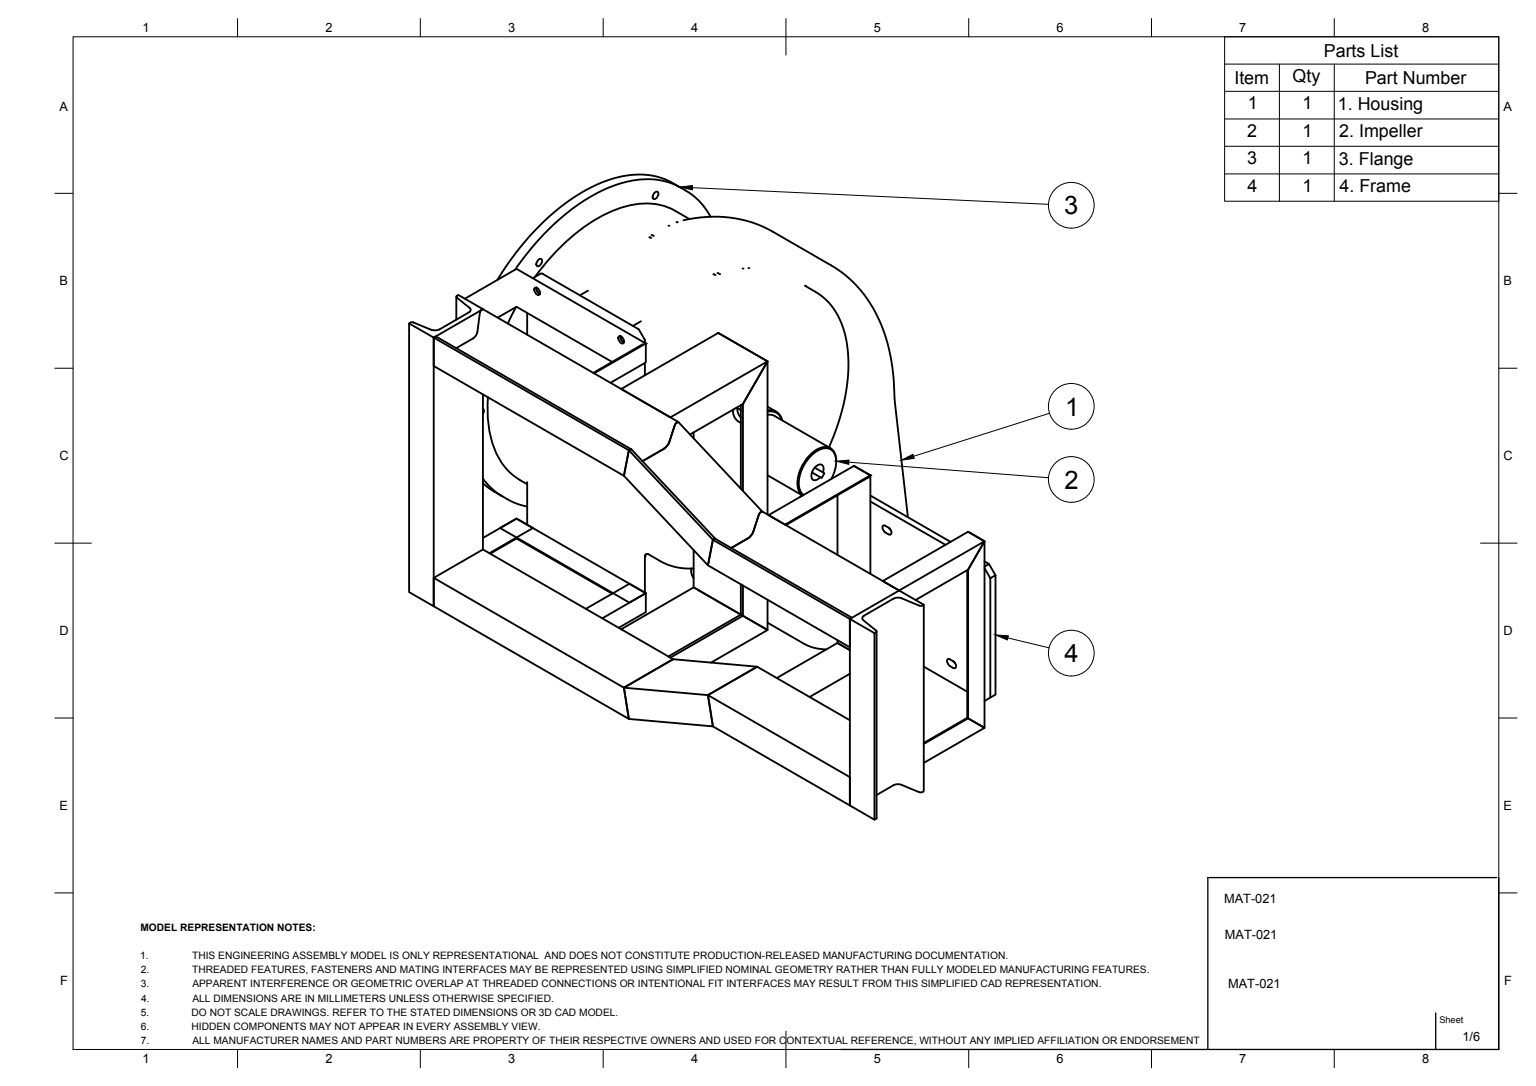
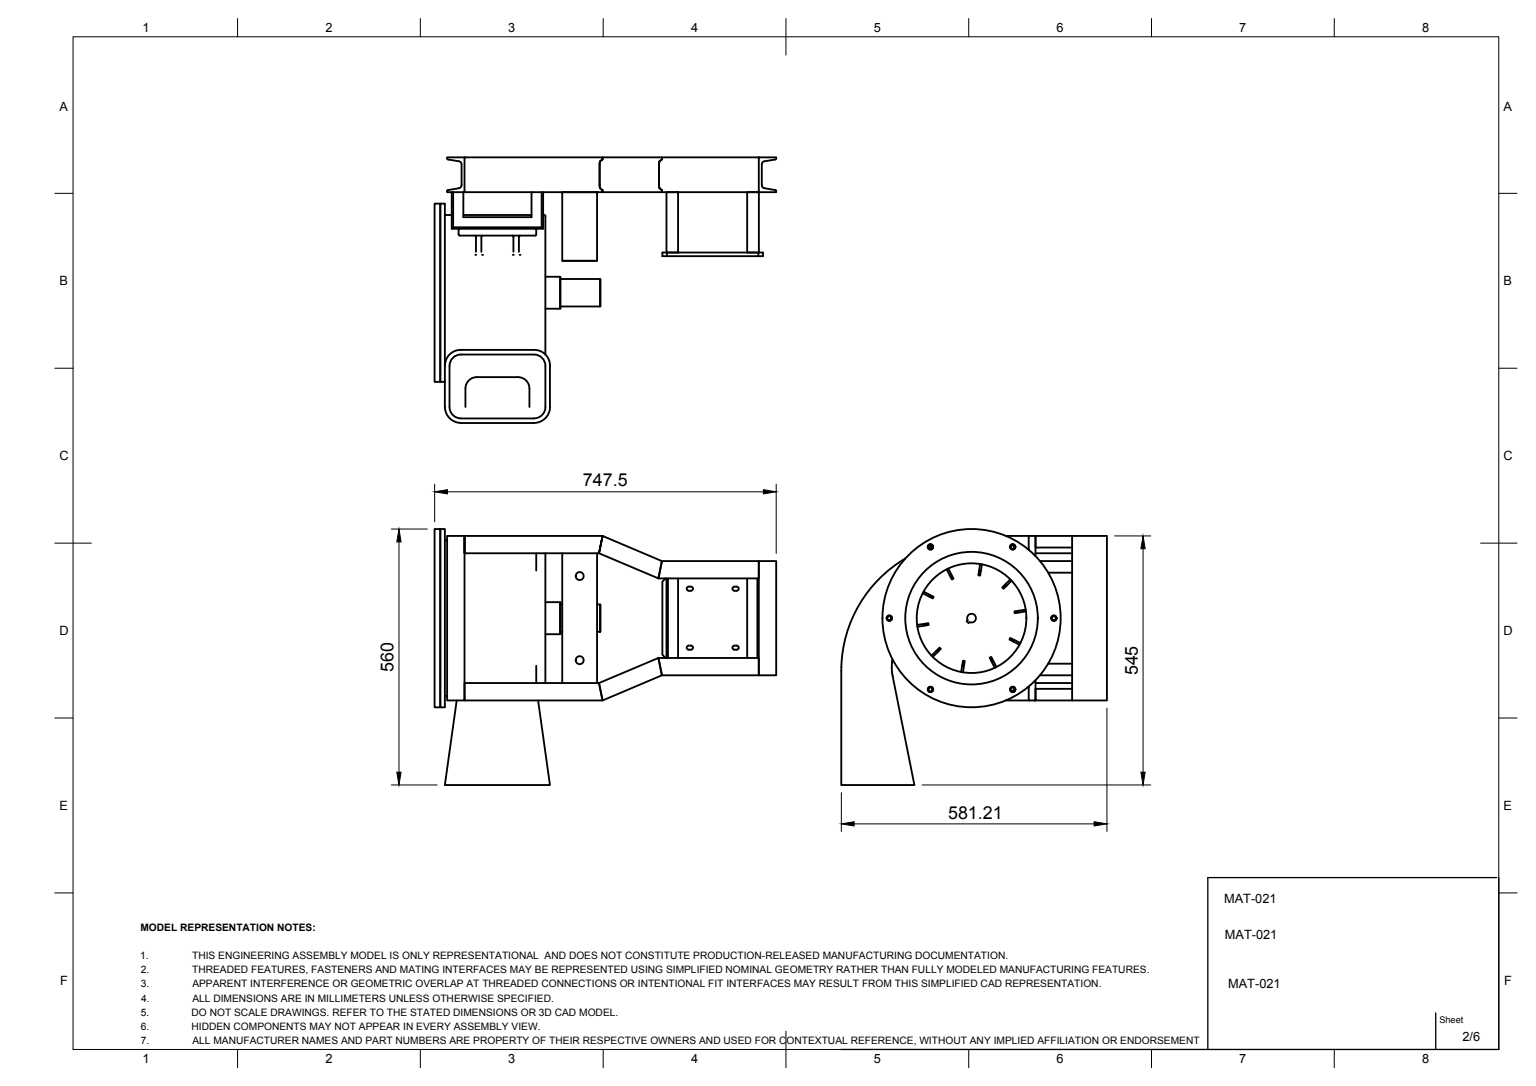
ISO-10303-21;
HEADER;
/* Generated by software containing ST-Developer
 * from STEP Tools, Inc. (www.steptools.com) 
 */

FILE_DESCRIPTION(
/* description */ ('STEP AP214'),
/* implementation_level */ '2;1');

FILE_NAME(
/* name */ 'MAT-021.step',
/* time_stamp */ '2026-11-14T06:27:21-08:00',
/* author */ (''),
/* organization */ (''),
/* preprocessor_version */ 'ST-DEVELOPER v20.2',
/* originating_system */ 'Autodesk Translation Framework v15.17.0.0',
/* authorisation */ '');

FILE_SCHEMA (('AUTOMOTIVE_DESIGN { 1 0 10303 214 3 1 1 }'));
ENDSEC;

DATA;
#10=MECHANICAL_DESIGN_GEOMETRIC_PRESENTATION_REPRESENTATION('',(#35,#36,
#37,#38,#39,#40,#41,#42,#43,#44,#45,#46,#47,#48,#49,#50,#51,#52,#53,#54,
#55,#56,#57,#58,#59,#60,#61),#27541);
#11=ITEM_DEFINED_TRANSFORMATION($,$,#11896,#13173);
#12=ITEM_DEFINED_TRANSFORMATION($,$,#12424,#13174);
#13=ITEM_DEFINED_TRANSFORMATION($,$,#12619,#13175);
#14=ITEM_DEFINED_TRANSFORMATION($,$,#12666,#13176);
#15=(
REPRESENTATION_RELATIONSHIP($,$,#27561,#27560)
REPRESENTATION_RELATIONSHIP_WITH_TRANSFORMATION(#11)
SHAPE_REPRESENTATION_RELATIONSHIP()
);
#16=(
REPRESENTATION_RELATIONSHIP($,$,#27562,#27560)
REPRESENTATION_RELATIONSHIP_WITH_TRANSFORMATION(#12)
SHAPE_REPRESENTATION_RELATIONSHIP()
);
#17=(
REPRESENTATION_RELATIONSHIP($,$,#27563,#27560)
REPRESENTATION_RELATIONSHIP_WITH_TRANSFORMATION(#13)
SHAPE_REPRESENTATION_RELATIONSHIP()
);
#18=(
REPRESENTATION_RELATIONSHIP($,$,#27564,#27560)
REPRESENTATION_RELATIONSHIP_WITH_TRANSFORMATION(#14)
SHAPE_REPRESENTATION_RELATIONSHIP()
);
#19=CONTEXT_DEPENDENT_SHAPE_REPRESENTATION(#15,#27556);
#20=CONTEXT_DEPENDENT_SHAPE_REPRESENTATION(#16,#27557);
#21=CONTEXT_DEPENDENT_SHAPE_REPRESENTATION(#17,#27558);
#22=CONTEXT_DEPENDENT_SHAPE_REPRESENTATION(#18,#27559);
#23=NEXT_ASSEMBLY_USAGE_OCCURRENCE('1. Housing:1','1. Housing:1',
'1. Housing:1',#27566,#27567,'1. Housing:1');
#24=NEXT_ASSEMBLY_USAGE_OCCURRENCE('2. Impeller:1','2. Impeller:1',
'2. Impeller:1',#27566,#27568,'2. Impeller:1');
#25=NEXT_ASSEMBLY_USAGE_OCCURRENCE('3. Flange:1','3. Flange:1',
'3. Flange:1',#27566,#27569,'3. Flange:1');
#26=NEXT_ASSEMBLY_USAGE_OCCURRENCE('4. Frame:1','4. Frame:1',
'4. Frame:1',#27566,#27570,'4. Frame:1');
#27=SHAPE_REPRESENTATION_RELATIONSHIP('SRR','None',#27561,#31);
#28=SHAPE_REPRESENTATION_RELATIONSHIP('SRR','None',#27562,#32);
#29=SHAPE_REPRESENTATION_RELATIONSHIP('SRR','None',#27563,#33);
#30=SHAPE_REPRESENTATION_RELATIONSHIP('SRR','None',#27564,#34);
#31=ADVANCED_BREP_SHAPE_REPRESENTATION('',(#62),#27537);
#32=ADVANCED_BREP_SHAPE_REPRESENTATION('',(#63),#27538);
#33=ADVANCED_BREP_SHAPE_REPRESENTATION('',(#64),#27539);
#34=ADVANCED_BREP_SHAPE_REPRESENTATION('',(#65,#66,#67,#68,#69,#70,#71,
#72,#73,#74,#75,#76,#77,#78,#79,#80,#81,#82,#83,#84,#85,#86,#87,#88),#27540);
#35=STYLED_ITEM('',(#27590),#62);
#36=STYLED_ITEM('',(#27591),#63);
#37=STYLED_ITEM('',(#27592),#64);
#38=STYLED_ITEM('',(#27590),#65);
#39=STYLED_ITEM('',(#27590),#66);
#40=STYLED_ITEM('',(#27590),#67);
#41=STYLED_ITEM('',(#27590),#68);
#42=STYLED_ITEM('',(#27590),#69);
#43=STYLED_ITEM('',(#27590),#70);
#44=STYLED_ITEM('',(#27590),#71);
#45=STYLED_ITEM('',(#27590),#72);
#46=STYLED_ITEM('',(#27590),#73);
#47=STYLED_ITEM('',(#27590),#74);
#48=STYLED_ITEM('',(#27590),#75);
#49=STYLED_ITEM('',(#27590),#76);
#50=STYLED_ITEM('',(#27590),#77);
#51=STYLED_ITEM('',(#27590),#78);
#52=STYLED_ITEM('',(#27590),#79);
#53=STYLED_ITEM('',(#27590),#80);
#54=STYLED_ITEM('',(#27590),#81);
#55=STYLED_ITEM('',(#27590),#82);
#56=STYLED_ITEM('',(#27590),#83);
#57=STYLED_ITEM('',(#27590),#84);
#58=STYLED_ITEM('',(#27590),#85);
#59=STYLED_ITEM('',(#27590),#86);
#60=STYLED_ITEM('',(#27590),#87);
#61=STYLED_ITEM('',(#27590),#88);
#62=MANIFOLD_SOLID_BREP('Body1',#11823);
#63=MANIFOLD_SOLID_BREP('Body1',#11824);
#64=MANIFOLD_SOLID_BREP('Body1',#11825);
#65=MANIFOLD_SOLID_BREP('Body1',#11826);
#66=MANIFOLD_SOLID_BREP('Body2',#11827);
#67=MANIFOLD_SOLID_BREP('Body3',#11828);
#68=MANIFOLD_SOLID_BREP('Body4',#11829);
#69=MANIFOLD_SOLID_BREP('Body5',#11830);
#70=MANIFOLD_SOLID_BREP('Body6',#11831);
#71=MANIFOLD_SOLID_BREP('Body7',#11832);
#72=MANIFOLD_SOLID_BREP('Body8',#11833);
#73=MANIFOLD_SOLID_BREP('Body9',#11834);
#74=MANIFOLD_SOLID_BREP('Body10',#11835);
#75=MANIFOLD_SOLID_BREP('Body11',#11836);
#76=MANIFOLD_SOLID_BREP('Body12',#11837);
#77=MANIFOLD_SOLID_BREP('Body13',#11838);
#78=MANIFOLD_SOLID_BREP('Body14',#11839);
#79=MANIFOLD_SOLID_BREP('Body15',#11840);
#80=MANIFOLD_SOLID_BREP('Body16',#11841);
#81=MANIFOLD_SOLID_BREP('Body17',#11842);
#82=MANIFOLD_SOLID_BREP('Body18',#11843);
#83=MANIFOLD_SOLID_BREP('Body19',#11844);
#84=MANIFOLD_SOLID_BREP('Body20',#11845);
#85=MANIFOLD_SOLID_BREP('Body21',#11846);
#86=MANIFOLD_SOLID_BREP('Body22',#11847);
#87=MANIFOLD_SOLID_BREP('Body23',#11848);
#88=MANIFOLD_SOLID_BREP('Body24',#11849);
#89=(
BOUNDED_SURFACE()
B_SPLINE_SURFACE(3,2,((#19385,#19386,#19387),(#19388,#19389,#19390),(#19391,
#19392,#19393),(#19394,#19395,#19396)),.UNSPECIFIED.,.F.,.F.,.F.)
B_SPLINE_SURFACE_WITH_KNOTS((4,4),(3,3),(4.8580615908835,4.90978454023457),
(0.,1.),.UNSPECIFIED.)
GEOMETRIC_REPRESENTATION_ITEM()
RATIONAL_B_SPLINE_SURFACE(((1.,0.714186893169771,1.),(1.,0.715014795561183,
1.),(1.,0.715838114785164,1.),(1.,0.716655802814478,1.)))
REPRESENTATION_ITEM('')
SURFACE()
);
#90=(
BOUNDED_SURFACE()
B_SPLINE_SURFACE(3,2,((#19398,#19399,#19400),(#19401,#19402,#19403),(#19404,
#19405,#19406),(#19407,#19408,#19409),(#19410,#19411,#19412),(#19413,#19414,
#19415)),.UNSPECIFIED.,.F.,.F.,.F.)
B_SPLINE_SURFACE_WITH_KNOTS((4,2,4),(3,3),(0.,0.00940850202008467,0.0188170040401693),
(0.,1.),.UNSPECIFIED.)
GEOMETRIC_REPRESENTATION_ITEM()
RATIONAL_B_SPLINE_SURFACE(((1.,0.707106781186548,1.),(1.,0.707160279657923,
1.),(1.,0.707792511111606,1.),(1.,0.710169444241066,1.),(1.,0.711914113489046,
1.),(1.,0.71418689316977,1.)))
REPRESENTATION_ITEM('')
SURFACE()
);
#91=(
BOUNDED_SURFACE()
B_SPLINE_SURFACE(3,2,((#19609,#19610,#19611),(#19612,#19613,#19614),(#19615,
#19616,#19617),(#19618,#19619,#19620)),.UNSPECIFIED.,.F.,.F.,.F.)
B_SPLINE_SURFACE_WITH_KNOTS((4,4),(3,3),(4.51499342053481,4.56671636988588),
(0.,1.),.UNSPECIFIED.)
GEOMETRIC_REPRESENTATION_ITEM()
RATIONAL_B_SPLINE_SURFACE(((1.,0.716655802814478,1.),(1.,0.715838114785163,
1.),(1.,0.715014795561185,1.),(1.,0.71418689316977,1.)))
REPRESENTATION_ITEM('')
SURFACE()
);
#92=(
BOUNDED_SURFACE()
B_SPLINE_SURFACE(3,2,((#19622,#19623,#19624),(#19625,#19626,#19627),(#19628,
#19629,#19630),(#19631,#19632,#19633),(#19634,#19635,#19636),(#19637,#19638,
#19639)),.UNSPECIFIED.,.F.,.F.,.F.)
B_SPLINE_SURFACE_WITH_KNOTS((4,2,4),(3,3),(0.,0.00940850202008465,0.0188170040401693),
(0.,1.),.UNSPECIFIED.)
GEOMETRIC_REPRESENTATION_ITEM()
RATIONAL_B_SPLINE_SURFACE(((1.,0.707106781186548,1.),(1.,0.707160279657923,
1.),(1.,0.707792511111607,1.),(1.,0.710169444241066,1.),(1.,0.711914113489046,
1.),(1.,0.714186893169771,1.)))
REPRESENTATION_ITEM('')
SURFACE()
);
#93=(
BOUNDED_SURFACE()
B_SPLINE_SURFACE(3,2,((#19835,#19836,#19837),(#19838,#19839,#19840),(#19841,
#19842,#19843),(#19844,#19845,#19846)),.UNSPECIFIED.,.F.,.F.,.F.)
B_SPLINE_SURFACE_WITH_KNOTS((4,4),(3,3),(0.,0.00696902930539232),(0.,1.),
 .UNSPECIFIED.)
GEOMETRIC_REPRESENTATION_ITEM()
RATIONAL_B_SPLINE_SURFACE(((1.,0.707106781186548,1.),(1.,0.707276293971192,
1.),(1.,0.707276133936197,1.),(1.,0.707106781186548,1.)))
REPRESENTATION_ITEM('')
SURFACE()
);
#94=(
BOUNDED_SURFACE()
B_SPLINE_SURFACE(3,2,((#20013,#20014,#20015),(#20016,#20017,#20018),(#20019,
#20020,#20021),(#20022,#20023,#20024)),.UNSPECIFIED.,.F.,.F.,.F.)
B_SPLINE_SURFACE_WITH_KNOTS((4,4),(3,3),(-3.46944695195361E-18,0.0069690293053924),
(0.,1.),.UNSPECIFIED.)
GEOMETRIC_REPRESENTATION_ITEM()
RATIONAL_B_SPLINE_SURFACE(((1.,0.707106781186547,1.),(1.,0.707276133936197,
1.),(1.,0.707276293971194,1.),(1.,0.707106781186547,1.)))
REPRESENTATION_ITEM('')
SURFACE()
);
#95=(
BOUNDED_SURFACE()
B_SPLINE_SURFACE(3,2,((#20196,#20197,#20198),(#20199,#20200,#20201),(#20202,
#20203,#20204),(#20205,#20206,#20207),(#20208,#20209,#20210),(#20211,#20212,
#20213),(#20214,#20215,#20216),(#20217,#20218,#20219),(#20220,#20221,#20222),
(#20223,#20224,#20225),(#20226,#20227,#20228),(#20229,#20230,#20231),(#20232,
#20233,#20234),(#20235,#20236,#20237),(#20238,#20239,#20240),(#20241,#20242,
#20243),(#20244,#20245,#20246),(#20247,#20248,#20249),(#20250,#20251,#20252),
(#20253,#20254,#20255),(#20256,#20257,#20258),(#20259,#20260,#20261),(#20262,
#20263,#20264),(#20265,#20266,#20267),(#20268,#20269,#20270),(#20271,#20272,
#20273),(#20274,#20275,#20276),(#20277,#20278,#20279),(#20280,#20281,#20282),
(#20283,#20284,#20285),(#20286,#20287,#20288),(#20289,#20290,#20291),(#20292,
#20293,#20294),(#20295,#20296,#20297),(#20298,#20299,#20300),(#20301,#20302,
#20303),(#20304,#20305,#20306),(#20307,#20308,#20309),(#20310,#20311,#20312),
(#20313,#20314,#20315),(#20316,#20317,#20318),(#20319,#20320,#20321)),
 .UNSPECIFIED.,.F.,.F.,.F.)
B_SPLINE_SURFACE_WITH_KNOTS((4,2,2,2,2,2,2,2,2,2,2,2,2,2,2,2,2,2,2,2,4),
(3,3),(-2.08303249130885E-5,0.0143336398395062,0.0286672796790123,0.0430009195185185,
0.0501677394382716,0.0573345593580246,0.0716681991975308,0.086001839037037,
0.100335478876543,0.10391888883642,0.107502298796296,0.114669118716049,
0.143336398395062,0.157670038234568,0.164836858154321,0.168420268114197,
0.172003678074074,0.200670957753086,0.215004597592592,0.222171417512345,
0.229338237432099),(-2.08303249131434E-5,1.),.UNSPECIFIED.)
GEOMETRIC_REPRESENTATION_ITEM()
RATIONAL_B_SPLINE_SURFACE(((1.0000122047894,0.707042750109083,1.),(1.00001165037919,
0.720350516962147,1.),(1.00001112382429,0.732989659531489,1.),(1.00001011791998,
0.757134849634084,1.),(1.00000963848844,0.768642868569314,1.),(1.00000871933328,
0.790705778250952,1.),(1.00000827963345,0.801260098384088,1.),(1.00000764642268,
0.816459351757556,1.),(1.00000743975533,0.821420084465031,1.),(1.00000703478498,
0.83114077643061,1.),(1.00000683745965,0.835877268408073,1.),(1.00000626125477,
0.849708182685712,1.),(1.00000589749541,0.858439668308409,1.),(1.00000520616899,
0.875033898554219,1.),(1.00000487861603,0.882896305052256,1.),(1.00000425655478,
0.897827931239669,1.),(1.00000396205458,0.904896956720407,1.),(1.00000361326943,
0.913269009275214,1.),(1.00000354448169,0.914920153464801,1.),(1.00000340882056,
0.918176490920243,1.),(1.00000334190225,0.919782762301647,1.),(1.00000314471007,
0.924516058194436,1.),(1.00000301778241,0.927562762018953,1.),(1.00000240476706,
0.942277255118144,1.),(1.00000198296934,0.952401862584738,1.),(1.0000014408388,
0.965414874578938,1.),(1.00000127533739,0.969387482068598,1.),(1.00000104925894,
0.974814148585356,1.),(1.00000097760072,0.976534194128842,1.),(1.0000008756353,
0.978981717570214,1.),(1.00000084253972,0.979776126225882,1.),(1.00000077837346,
0.981316338884772,1.),(1.00000074729348,0.982062366173435,1.),(1.00000047647086,
0.988563047871222,1.),(1.0000002985221,0.992834434768701,1.),(1.00000011982054,
0.997123891622385,1.),(1.00000007504731,0.998198604512223,1.),(1.00000003010649,
0.999277339877407,1.),(1.00000001883456,0.999547905223287,1.),(1.00000000377558,
0.999909373055038,1.),(0.999999999994412,1.00000013413799,1.),(1.,1.,1.)))
REPRESENTATION_ITEM('')
SURFACE()
);
#96=(
BOUNDED_SURFACE()
B_SPLINE_SURFACE(3,2,((#20325,#20326,#20327),(#20328,#20329,#20330),(#20331,
#20332,#20333),(#20334,#20335,#20336),(#20337,#20338,#20339),(#20340,#20341,
#20342),(#20343,#20344,#20345),(#20346,#20347,#20348),(#20349,#20350,#20351),
(#20352,#20353,#20354),(#20355,#20356,#20357),(#20358,#20359,#20360),(#20361,
#20362,#20363),(#20364,#20365,#20366),(#20367,#20368,#20369),(#20370,#20371,
#20372),(#20373,#20374,#20375),(#20376,#20377,#20378),(#20379,#20380,#20381),
(#20382,#20383,#20384),(#20385,#20386,#20387),(#20388,#20389,#20390),(#20391,
#20392,#20393),(#20394,#20395,#20396),(#20397,#20398,#20399),(#20400,#20401,
#20402),(#20403,#20404,#20405),(#20406,#20407,#20408),(#20409,#20410,#20411),
(#20412,#20413,#20414),(#20415,#20416,#20417),(#20418,#20419,#20420),(#20421,
#20422,#20423),(#20424,#20425,#20426),(#20427,#20428,#20429),(#20430,#20431,
#20432),(#20433,#20434,#20435),(#20436,#20437,#20438),(#20439,#20440,#20441),
(#20442,#20443,#20444),(#20445,#20446,#20447),(#20448,#20449,#20450),(#20451,
#20452,#20453),(#20454,#20455,#20456)),.UNSPECIFIED.,.F.,.F.,.F.)
B_SPLINE_SURFACE_WITH_KNOTS((4,2,2,2,2,2,2,2,2,2,2,2,2,2,2,2,2,2,2,2,2,
4),(3,3),(0.,0.0134129175527026,0.0268258351054052,0.0335322938817565,0.0368855232699322,
0.0402387526581078,0.0469452114344592,0.0536516702108105,0.0603581289871618,
0.0637113583753374,0.0670645877635131,0.0737710465398644,0.0804775053162157,
0.0838307347043914,0.087183964092567,0.0905371934807427,0.0938904228689183,
0.0955670375630061,0.097243652257094,0.10059688164527,0.103950111033445,
0.107303340421621),(0.,1.),.UNSPECIFIED.)
GEOMETRIC_REPRESENTATION_ITEM()
RATIONAL_B_SPLINE_SURFACE(((1.,0.707106781186548,1.),(1.,0.692435075400818,
1.),(1.,0.677415299381314,1.),(1.,0.646471084851157,1.),(1.,0.63054857897306,
1.),(1.,0.605783714123967,1.),(1.,0.597381263170599,1.),(1.,0.584523409966303,
1.),(1.,0.580195037882829,1.),(1.,0.571447189603745,1.),(1.,0.56702021135895,
1.),(1.,0.553648440044157,1.),(1.,0.544640272160397,1.),(1.,0.526415110072128,
1.),(1.,0.51719794329847,1.),(1.,0.498539063660432,1.),(1.,0.489096977102246,
1.),(1.,0.474763871347392,1.),(1.,0.469957977677047,1.),(1.,0.460292200732756,
1.),(1.,0.455439380592845,1.),(1.,0.440953583986291,1.),(1.,0.431346601606819,
1.),(1.,0.412377017907544,1.),(1.,0.403011528923584,1.),(1.,0.389351796591827,
1.),(1.,0.384854537462147,1.),(1.,0.376177060931741,1.),(1.,0.371982004193461,
1.),(1.,0.363944301803223,1.),(1.,0.360101535707161,1.),(1.,0.352850425245751,
1.),(1.,0.349441929276512,1.),(1.,0.344732409186674,1.),(1.,0.343226443951063,
1.),(1.,0.340393341785211,1.),(1.,0.339063346120003,1.),(1.,0.335345379291585,
1.),(1.,0.333229400572389,1.),(1.,0.329790328424277,1.),(1.,0.328467328740303,
1.),(1.,0.326681697649074,1.),(1.,0.326219073225421,1.),(1.,0.326219127150631,
1.)))
REPRESENTATION_ITEM('')
SURFACE()
);
#97=(
BOUNDED_SURFACE()
B_SPLINE_SURFACE(3,2,((#20457,#20458,#20459),(#20460,#20461,#20462),(#20463,
#20464,#20465),(#20466,#20467,#20468),(#20469,#20470,#20471),(#20472,#20473,
#20474),(#20475,#20476,#20477),(#20478,#20479,#20480),(#20481,#20482,#20483),
(#20484,#20485,#20486),(#20487,#20488,#20489),(#20490,#20491,#20492),(#20493,
#20494,#20495),(#20496,#20497,#20498),(#20499,#20500,#20501),(#20502,#20503,
#20504),(#20505,#20506,#20507),(#20508,#20509,#20510),(#20511,#20512,#20513),
(#20514,#20515,#20516),(#20517,#20518,#20519),(#20520,#20521,#20522),(#20523,
#20524,#20525),(#20526,#20527,#20528),(#20529,#20530,#20531),(#20532,#20533,
#20534),(#20535,#20536,#20537),(#20538,#20539,#20540),(#20541,#20542,#20543),
(#20544,#20545,#20546),(#20547,#20548,#20549),(#20550,#20551,#20552),(#20553,
#20554,#20555),(#20556,#20557,#20558),(#20559,#20560,#20561),(#20562,#20563,
#20564),(#20565,#20566,#20567),(#20568,#20569,#20570),(#20571,#20572,#20573),
(#20574,#20575,#20576),(#20577,#20578,#20579),(#20580,#20581,#20582),(#20583,
#20584,#20585),(#20586,#20587,#20588),(#20589,#20590,#20591),(#20592,#20593,
#20594)),.UNSPECIFIED.,.F.,.F.,.F.)
B_SPLINE_SURFACE_WITH_KNOTS((4,2,2,2,2,2,2,2,2,2,2,2,2,2,2,2,2,2,2,2,2,
2,4),(3,3),(0.,0.00337857504716453,0.00675715009432906,0.0101357251414936,
0.0118250126650759,0.0135143001886581,0.0168928752358226,0.0202714502829872,
0.0236500253301517,0.025339312853734,0.0270286003773162,0.0337857504716453,
0.0405429005659744,0.0439214756131389,0.0473000506603034,0.0540572007546325,
0.0608143508489615,0.0675715009432906,0.0709500759904551,0.0743286510376197,
0.0810858011319487,0.0946001013206068,0.108114401509265),(0.,1.),
 .UNSPECIFIED.)
GEOMETRIC_REPRESENTATION_ITEM()
RATIONAL_B_SPLINE_SURFACE(((1.,0.32621912715063,1.),(1.,0.326219068852315,
1.),(1.,0.326681715050001,1.),(1.,0.328468620211654,1.),(1.,0.32979287514018,
1.),(1.,0.333236641150815,1.),(1.,0.33535605687756,1.),(1.,0.339081365168914,
1.),(1.,0.340414170801098,1.),(1.,0.34325369454111,1.),(1.,0.344759275422739,
1.),(1.,0.349467998468122,1.),(1.,0.352877852486234,1.),(1.,0.360137129421262,
1.),(1.,0.363986689978637,1.),(1.,0.372044278816161,1.),(1.,0.37625241873187,
1.),(1.,0.382785172371532,1.),(1.,0.385002445825604,1.),(1.,0.389470383554178,
1.),(1.,0.391724641087319,1.),(1.,0.403081163733532,1.),(1.,0.412431784451128,
1.),(1.,0.431385484934698,1.),(1.,0.440991365631289,1.),(1.,0.455485214499389,
1.),(1.,0.460343755015816,1.),(1.,0.469998884973711,1.),(1.,0.474798889815344,
1.),(1.,0.48911283545623,1.),(1.,0.498540168051125,1.),(1.,0.517166334136202,
1.),(1.,0.526365537230034,1.),(1.,0.544552008443698,1.),(1.,0.553539446694172,
1.),(1.,0.566878228388953,1.),(1.,0.571308885947455,1.),(1.,0.580076325189919,
1.),(1.,0.584413767367782,1.),(1.,0.597296867359364,1.),(1.,0.605713540127583,
1.),(1.,0.630514573129104,1.),(1.,0.646452607022068,1.),(1.,0.677415122211174,
1.),(1.,0.692437606205447,1.),(1.,0.707106781186548,1.)))
REPRESENTATION_ITEM('')
SURFACE()
);
#98=(
BOUNDED_SURFACE()
B_SPLINE_SURFACE(3,2,((#20598,#20599,#20600),(#20601,#20602,#20603),(#20604,
#20605,#20606),(#20607,#20608,#20609),(#20610,#20611,#20612),(#20613,#20614,
#20615),(#20616,#20617,#20618),(#20619,#20620,#20621),(#20622,#20623,#20624),
(#20625,#20626,#20627),(#20628,#20629,#20630),(#20631,#20632,#20633),(#20634,
#20635,#20636),(#20637,#20638,#20639),(#20640,#20641,#20642),(#20643,#20644,
#20645),(#20646,#20647,#20648),(#20649,#20650,#20651),(#20652,#20653,#20654),
(#20655,#20656,#20657),(#20658,#20659,#20660),(#20661,#20662,#20663),(#20664,
#20665,#20666),(#20667,#20668,#20669),(#20670,#20671,#20672),(#20673,#20674,
#20675),(#20676,#20677,#20678),(#20679,#20680,#20681),(#20682,#20683,#20684),
(#20685,#20686,#20687),(#20688,#20689,#20690),(#20691,#20692,#20693),(#20694,
#20695,#20696),(#20697,#20698,#20699),(#20700,#20701,#20702),(#20703,#20704,
#20705),(#20706,#20707,#20708),(#20709,#20710,#20711),(#20712,#20713,#20714),
(#20715,#20716,#20717),(#20718,#20719,#20720),(#20721,#20722,#20723)),
 .UNSPECIFIED.,.F.,.F.,.F.)
B_SPLINE_SURFACE_WITH_KNOTS((4,2,2,2,2,2,2,2,2,2,2,2,2,2,2,2,2,2,2,2,4),
(3,3),(-2.08246099844738E-5,0.0143336398395062,0.0286672796790123,0.0430009195185185,
0.0501677394382716,0.0573345593580247,0.0716681991975308,0.086001839037037,
0.100335478876543,0.10391888883642,0.107502298796296,0.114669118716049,
0.143336398395062,0.157670038234568,0.164836858154321,0.168420268114197,
0.172003678074074,0.200670957753086,0.215004597592593,0.222171417512346,
0.229338237432099),(0.,1.00002082460998),.UNSPECIFIED.)
GEOMETRIC_REPRESENTATION_ITEM()
RATIONAL_B_SPLINE_SURFACE(((1.,0.707042767677887,1.00001220144021),(1.,
0.720350528626315,1.00001164718235),(1.,0.732989665864678,1.00001112077214),
(1.,0.757134851024669,1.00001011514401),(1.,0.768642869892271,1.000009635844),
(1.,0.790705779446232,1.00000871694103),(1.,0.801260099519581,1.00000827736183),
(1.,0.816459352806589,1.00000764432479),(1.,0.821420085485447,1.00000743771414),
(1.,0.831140777395743,1.00000703285491),(1.,0.835877269346536,1.00000683558371),
(1.,0.849708183543533,1.00000625953692),(1.,0.85843966911793,1.00000589587736),
(1.,0.875033899267846,1.00000520474062),(1.,0.882896305722012,1.00000487727752),
(1.,0.897827931823032,1.00000425538694),(1.,0.904896957262567,1.00000396096755),
(1.,0.913269009771199,1.00000361227809),(1.,0.914920153950816,1.00000354350922),
(1.,0.918176491388049,1.00000340788531),(1.,0.919782762760141,1.00000334098536),
(1.,0.924516058625678,1.00000314384728),(1.,0.927562762433317,1.00000301695444),
(1.,0.94227725544642,1.00000240410729),(1.,0.952401862855693,1.00000198242528),
(1.,0.965414874777115,1.00000144044349),(1.,0.969387482243809,1.00000127498749),
(1.,0.974814148729155,1.00000104897106),(1.,0.976534194262543,1.0000009773325),
(1.,0.97898171769053,1.00000087539506),(1.,0.979776126341324,1.00000084230856),
(1.,0.981316338991679,1.00000077815991),(1.,0.982062366275678,1.00000074708845),
(1.,0.988563047938719,1.00000047634013),(1.,0.992834434811244,1.0000002984402),
(1.,0.997123891638026,1.00000011978767),(1.,0.998198604522518,1.00000007502672),
(1.,0.999277339881537,1.00000003009823),(1.,0.999547905226004,1.00000001882939),
(1.,0.999909373055422,1.00000000377454),(1.,1.00000013413809,0.999999999994413),
(1.,1.,1.)))
REPRESENTATION_ITEM('')
SURFACE()
);
#99=(
BOUNDED_SURFACE()
B_SPLINE_SURFACE(3,2,((#20852,#20853,#20854),(#20855,#20856,#20857),(#20858,
#20859,#20860),(#20861,#20862,#20863)),.UNSPECIFIED.,.F.,.F.,.F.)
B_SPLINE_SURFACE_WITH_KNOTS((4,4),(3,3),(4.8580615908835,4.90978454023457),
(0.,1.),.UNSPECIFIED.)
GEOMETRIC_REPRESENTATION_ITEM()
RATIONAL_B_SPLINE_SURFACE(((1.,0.714186893169771,1.),(1.,0.715014795561184,
1.),(1.,0.715838114785164,1.),(1.,0.716655802814478,1.)))
REPRESENTATION_ITEM('')
SURFACE()
);
#100=(
BOUNDED_SURFACE()
B_SPLINE_SURFACE(3,2,((#20865,#20866,#20867),(#20868,#20869,#20870),(#20871,
#20872,#20873),(#20874,#20875,#20876),(#20877,#20878,#20879),(#20880,#20881,
#20882)),.UNSPECIFIED.,.F.,.F.,.F.)
B_SPLINE_SURFACE_WITH_KNOTS((4,2,4),(3,3),(0.,0.00940850202008467,0.0188170040401693),
(0.,1.),.UNSPECIFIED.)
GEOMETRIC_REPRESENTATION_ITEM()
RATIONAL_B_SPLINE_SURFACE(((1.,0.707106781186548,1.),(1.,0.707160279657923,
1.),(1.,0.707792511111606,1.),(1.,0.710169444241066,1.),(1.,0.711914113489048,
1.),(1.,0.714186893169771,1.)))
REPRESENTATION_ITEM('')
SURFACE()
);
#101=(
BOUNDED_SURFACE()
B_SPLINE_SURFACE(3,2,((#21103,#21104,#21105),(#21106,#21107,#21108),(#21109,
#21110,#21111),(#21112,#21113,#21114)),.UNSPECIFIED.,.F.,.F.,.F.)
B_SPLINE_SURFACE_WITH_KNOTS((4,4),(3,3),(4.51499342053481,4.56671636988588),
(0.,1.),.UNSPECIFIED.)
GEOMETRIC_REPRESENTATION_ITEM()
RATIONAL_B_SPLINE_SURFACE(((1.,0.716655802814478,1.),(1.,0.715838114785163,
1.),(1.,0.715014795561185,1.),(1.,0.71418689316977,1.)))
REPRESENTATION_ITEM('')
SURFACE()
);
#102=(
BOUNDED_SURFACE()
B_SPLINE_SURFACE(3,2,((#21116,#21117,#21118),(#21119,#21120,#21121),(#21122,
#21123,#21124),(#21125,#21126,#21127),(#21128,#21129,#21130),(#21131,#21132,
#21133)),.UNSPECIFIED.,.F.,.F.,.F.)
B_SPLINE_SURFACE_WITH_KNOTS((4,2,4),(3,3),(-1.38777878078145E-17,0.00940850202008464,
0.0188170040401693),(0.,1.),.UNSPECIFIED.)
GEOMETRIC_REPRESENTATION_ITEM()
RATIONAL_B_SPLINE_SURFACE(((1.,0.707106781186548,1.),(1.,0.707160279657923,
1.),(1.,0.707792511111607,1.),(1.,0.710169444241066,1.),(1.,0.711914113489046,
1.),(1.,0.714186893169771,1.)))
REPRESENTATION_ITEM('')
SURFACE()
);
#103=(
BOUNDED_SURFACE()
B_SPLINE_SURFACE(3,2,((#21362,#21363,#21364),(#21365,#21366,#21367),(#21368,
#21369,#21370),(#21371,#21372,#21373)),.UNSPECIFIED.,.F.,.F.,.F.)
B_SPLINE_SURFACE_WITH_KNOTS((4,4),(3,3),(0.,0.00696902930539231),(0.,1.),
 .UNSPECIFIED.)
GEOMETRIC_REPRESENTATION_ITEM()
RATIONAL_B_SPLINE_SURFACE(((1.,0.707106781186548,1.),(1.,0.707276293971192,
1.),(1.,0.707276133936197,1.),(1.,0.707106781186548,1.)))
REPRESENTATION_ITEM('')
SURFACE()
);
#104=(
BOUNDED_SURFACE()
B_SPLINE_SURFACE(3,2,((#21540,#21541,#21542),(#21543,#21544,#21545),(#21546,
#21547,#21548),(#21549,#21550,#21551)),.UNSPECIFIED.,.F.,.F.,.F.)
B_SPLINE_SURFACE_WITH_KNOTS((4,4),(3,3),(-3.46944695195361E-18,0.0069690293053924),
(0.,1.),.UNSPECIFIED.)
GEOMETRIC_REPRESENTATION_ITEM()
RATIONAL_B_SPLINE_SURFACE(((1.,0.707106781186547,1.),(1.,0.707276133936196,
1.),(1.,0.707276293971194,1.),(1.,0.707106781186547,1.)))
REPRESENTATION_ITEM('')
SURFACE()
);
#105=(
BOUNDED_SURFACE()
B_SPLINE_SURFACE(3,2,((#21711,#21712,#21713),(#21714,#21715,#21716),(#21717,
#21718,#21719),(#21720,#21721,#21722),(#21723,#21724,#21725),(#21726,#21727,
#21728),(#21729,#21730,#21731),(#21732,#21733,#21734),(#21735,#21736,#21737),
(#21738,#21739,#21740),(#21741,#21742,#21743),(#21744,#21745,#21746),(#21747,
#21748,#21749),(#21750,#21751,#21752),(#21753,#21754,#21755),(#21756,#21757,
#21758),(#21759,#21760,#21761),(#21762,#21763,#21764),(#21765,#21766,#21767),
(#21768,#21769,#21770),(#21771,#21772,#21773),(#21774,#21775,#21776),(#21777,
#21778,#21779),(#21780,#21781,#21782),(#21783,#21784,#21785),(#21786,#21787,
#21788),(#21789,#21790,#21791),(#21792,#21793,#21794),(#21795,#21796,#21797),
(#21798,#21799,#21800),(#21801,#21802,#21803),(#21804,#21805,#21806),(#21807,
#21808,#21809),(#21810,#21811,#21812),(#21813,#21814,#21815),(#21816,#21817,
#21818),(#21819,#21820,#21821),(#21822,#21823,#21824),(#21825,#21826,#21827),
(#21828,#21829,#21830),(#21831,#21832,#21833),(#21834,#21835,#21836)),
 .UNSPECIFIED.,.F.,.F.,.F.)
B_SPLINE_SURFACE_WITH_KNOTS((4,2,2,2,2,2,2,2,2,2,2,2,2,2,2,2,2,2,2,2,4),
(3,3),(-1.33632684703268E-5,0.0143336398395061,0.0286672796790123,0.0430009195185185,
0.0501677394382715,0.0573345593580246,0.0716681991975308,0.086001839037037,
0.100335478876543,0.10391888883642,0.107502298796296,0.114669118716049,
0.143336398395062,0.157670038234568,0.164836858154321,0.168420268114197,
0.172003678074074,0.200670957753086,0.215004597592592,0.222171417512345,
0.229338237432099),(-1.33632684703573E-5,1.),.UNSPECIFIED.)
GEOMETRIC_REPRESENTATION_ITEM()
RATIONAL_B_SPLINE_SURFACE(((1.00000782911927,0.707065704608532,1.),(1.000007473655,
0.72036575434847,1.),(1.00000713604048,0.732997937829732,1.),(1.00000649089595,
0.757136663085689,1.),(1.00000618332875,0.768644596089292,1.),(1.00000559366798,
0.790707341030961,1.),(1.00000531158966,0.801261582354705,1.),(1.00000490536929,
0.816460722237655,1.),(1.00000477278707,0.821421417903966,1.),(1.00000451298858,
0.831142037285297,1.),(1.0000043863995,0.835878493896513,1.),(1.00000401674981,
0.849709304899285,1.),(1.00000378338918,0.858440725325112,1.),(1.00000333988619,
0.875034831663981,1.),(1.00000312975286,0.882897179455003,1.),(1.00000273068518,
0.89782869414732,1.),(1.00000254175602,0.904897666844873,1.),(1.00000231800172,
0.913269656887061,1.),(1.00000227387268,0.914920788747183,1.),(1.00000218684271,
0.918177101888678,1.),(1.00000214391296,0.919783361275745,1.),(1.0000020174093,
0.924516621825683,1.),(1.00000193598206,0.92756330290103,1.),(1.00000154271755,
0.942277686126561,1.),(1.00000127212388,0.952402217994254,1.),(1.00000092433373,
0.965415132823172,1.),(1.00000081816048,0.969387710649768,1.),(1.00000067312556,
0.974814336645346,1.),(1.00000062715504,0.976534369345689,1.),(1.00000056174171,
0.978981874511646,1.),(1.00000054051007,0.979776277235544,1.),(1.00000049934583,
0.981316478393818,1.),(1.00000047940725,0.982062500111768,1.),(1.00000030566784,
0.988563133271413,1.),(1.00000019150931,0.992834488272736,1.),(1.00000007686784,
0.997123913098267,1.),(1.0000000481447,0.998198617963065,1.),(1.00000001931406,
0.999277345273439,1.),(1.00000001208284,0.999547908599034,1.),(1.00000000242213,
0.99990937373174,1.),(0.999999999996415,1.00000013413699,1.),(1.,1.,1.)))
REPRESENTATION_ITEM('')
SURFACE()
);
#106=(
BOUNDED_SURFACE()
B_SPLINE_SURFACE(3,2,((#21840,#21841,#21842),(#21843,#21844,#21845),(#21846,
#21847,#21848),(#21849,#21850,#21851),(#21852,#21853,#21854),(#21855,#21856,
#21857),(#21858,#21859,#21860),(#21861,#21862,#21863),(#21864,#21865,#21866),
(#21867,#21868,#21869),(#21870,#21871,#21872),(#21873,#21874,#21875),(#21876,
#21877,#21878),(#21879,#21880,#21881),(#21882,#21883,#21884),(#21885,#21886,
#21887),(#21888,#21889,#21890),(#21891,#21892,#21893),(#21894,#21895,#21896),
(#21897,#21898,#21899),(#21900,#21901,#21902),(#21903,#21904,#21905),(#21906,
#21907,#21908),(#21909,#21910,#21911),(#21912,#21913,#21914),(#21915,#21916,
#21917),(#21918,#21919,#21920),(#21921,#21922,#21923),(#21924,#21925,#21926),
(#21927,#21928,#21929),(#21930,#21931,#21932),(#21933,#21934,#21935),(#21936,
#21937,#21938),(#21939,#21940,#21941),(#21942,#21943,#21944),(#21945,#21946,
#21947),(#21948,#21949,#21950),(#21951,#21952,#21953),(#21954,#21955,#21956),
(#21957,#21958,#21959),(#21960,#21961,#21962),(#21963,#21964,#21965),(#21966,
#21967,#21968),(#21969,#21970,#21971),(#21972,#21973,#21974),(#21975,#21976,
#21977)),.UNSPECIFIED.,.F.,.F.,.F.)
B_SPLINE_SURFACE_WITH_KNOTS((4,2,2,2,2,2,2,2,2,2,2,2,2,2,2,2,2,2,2,2,2,
2,4),(3,3),(0.,0.0134129175527026,0.0268258351054052,0.0335322938817565,
0.0368855232699322,0.0402387526581078,0.0469452114344592,0.0536516702108105,
0.0603581289871618,0.0637113583753374,0.0670645877635131,0.0737710465398644,
0.07712427592804,0.0804775053162157,0.0838307347043914,0.087183964092567,
0.0905371934807427,0.0938904228689183,0.0955670375630061,0.097243652257094,
0.10059688164527,0.103950111033445,0.107303340421621),(0.,1.),
 .UNSPECIFIED.)
GEOMETRIC_REPRESENTATION_ITEM()
RATIONAL_B_SPLINE_SURFACE(((1.,0.707106781186548,1.),(1.,0.692435075401192,
1.),(1.,0.677415299380816,1.),(1.,0.646471084851654,1.),(1.,0.630548578972812,
1.),(1.,0.605783714124091,1.),(1.,0.597381263170474,1.),(1.,0.584523409966366,
1.),(1.,0.580195037882892,1.),(1.,0.571447189603682,1.),(1.,0.56702021135914,
1.),(1.,0.553648440043779,1.),(1.,0.544640272160396,1.),(1.,0.526415110072127,
1.),(1.,0.517197943298344,1.),(1.,0.498539063660557,1.),(1.,0.489096977102497,
1.),(1.,0.474763871347267,1.),(1.,0.469957977677141,1.),(1.,0.460292200732662,
1.),(1.,0.455439380593066,1.),(1.,0.440953583985851,1.),(1.,0.431346601607069,
1.),(1.,0.417119413832237,1.),(1.,0.412408247679678,1.),(1.,0.403077747649425,
1.),(1.,0.398458284812998,1.),(1.,0.389351796591827,1.),(1.,0.384854537462053,
1.),(1.,0.376177060931835,1.),(1.,0.371982004193336,1.),(1.,0.363944301803349,
1.),(1.,0.360101535706815,1.),(1.,0.352850425246096,1.),(1.,0.349441929276512,
1.),(1.,0.344732409186674,1.),(1.,0.343226443951127,1.),(1.,0.340393341785148,
1.),(1.,0.339063346120349,1.),(1.,0.335345379290893,1.),(1.,0.333229400572264,
1.),(1.,0.329790328424402,1.),(1.,0.328467328740178,1.),(1.,0.326681697649199,
1.),(1.,0.326219073225326,1.),(1.,0.326219127150631,1.)))
REPRESENTATION_ITEM('')
SURFACE()
);
#107=(
BOUNDED_SURFACE()
B_SPLINE_SURFACE(3,2,((#21978,#21979,#21980),(#21981,#21982,#21983),(#21984,
#21985,#21986),(#21987,#21988,#21989),(#21990,#21991,#21992),(#21993,#21994,
#21995),(#21996,#21997,#21998),(#21999,#22000,#22001),(#22002,#22003,#22004),
(#22005,#22006,#22007),(#22008,#22009,#22010),(#22011,#22012,#22013),(#22014,
#22015,#22016),(#22017,#22018,#22019),(#22020,#22021,#22022),(#22023,#22024,
#22025),(#22026,#22027,#22028),(#22029,#22030,#22031),(#22032,#22033,#22034),
(#22035,#22036,#22037),(#22038,#22039,#22040),(#22041,#22042,#22043),(#22044,
#22045,#22046),(#22047,#22048,#22049),(#22050,#22051,#22052),(#22053,#22054,
#22055),(#22056,#22057,#22058),(#22059,#22060,#22061),(#22062,#22063,#22064),
(#22065,#22066,#22067),(#22068,#22069,#22070),(#22071,#22072,#22073),(#22074,
#22075,#22076),(#22077,#22078,#22079),(#22080,#22081,#22082),(#22083,#22084,
#22085),(#22086,#22087,#22088),(#22089,#22090,#22091),(#22092,#22093,#22094),
(#22095,#22096,#22097),(#22098,#22099,#22100),(#22101,#22102,#22103),(#22104,
#22105,#22106),(#22107,#22108,#22109),(#22110,#22111,#22112),(#22113,#22114,
#22115),(#22116,#22117,#22118),(#22119,#22120,#22121)),.UNSPECIFIED.,.F.,
 .F.,.F.)
B_SPLINE_SURFACE_WITH_KNOTS((4,2,2,2,2,2,2,2,2,2,2,2,2,2,2,2,2,2,2,2,2,
2,2,4),(3,3),(0.,0.00337857504716453,0.00675715009432906,0.0101357251414936,
0.0118250126650759,0.0135143001886581,0.0168928752358226,0.0202714502829872,
0.0236500253301517,0.025339312853734,0.0270286003773162,0.0304071754244808,
0.0337857504716453,0.0405429005659744,0.0439214756131389,0.0473000506603034,
0.0540572007546325,0.0608143508489615,0.0675715009432906,0.0709500759904551,
0.0743286510376197,0.0810858011319487,0.0946001013206068,0.108114401509265),
(0.,1.),.UNSPECIFIED.)
GEOMETRIC_REPRESENTATION_ITEM()
RATIONAL_B_SPLINE_SURFACE(((1.,0.32621912715063,1.),(1.,0.326219068852551,
1.),(1.,0.326681715049687,1.),(1.,0.328468620211968,1.),(1.,0.329792875139961,
1.),(1.,0.333236641151033,1.),(1.,0.33535605687756,1.),(1.,0.339081365168914,
1.),(1.,0.340414170800971,1.),(1.,0.343253694541237,1.),(1.,0.344759275422691,
1.),(1.,0.349467998468217,1.),(1.,0.352877852486455,1.),(1.,0.360137129421043,
1.),(1.,0.363986689978511,1.),(1.,0.372044278816287,1.),(1.,0.37625241873225,
1.),(1.,0.382785172371342,1.),(1.,0.385002445825604,1.),(1.,0.389470383554178,
1.),(1.,0.391724641087209,1.),(1.,0.398538554675267,1.),(1.,0.403148955697984,
1.),(1.,0.412464720989499,1.),(1.,0.417170209572146,1.),(1.,0.431385484934447,
1.),(1.,0.44099136563173,1.),(1.,0.455485214499169,1.),(1.,0.460343755015469,
1.),(1.,0.469998884974058,1.),(1.,0.474798889815438,1.),(1.,0.489112835456042,
1.),(1.,0.498540168051997,1.),(1.,0.517166334135328,1.),(1.,0.526365537230033,
1.),(1.,0.544552008443698,1.),(1.,0.553539446694675,1.),(1.,0.566878228388702,
1.),(1.,0.571308885947581,1.),(1.,0.580076325189793,1.),(1.,0.584413767367218,
1.),(1.,0.597296867360491,1.),(1.,0.605713540127086,1.),(1.,0.630514573130101,
1.),(1.,0.646452607020576,1.),(1.,0.677415122212667,1.),(1.,0.692437606204326,
1.),(1.,0.707106781186548,1.)))
REPRESENTATION_ITEM('')
SURFACE()
);
#108=(
BOUNDED_SURFACE()
B_SPLINE_SURFACE(3,2,((#22125,#22126,#22127),(#22128,#22129,#22130),(#22131,
#22132,#22133),(#22134,#22135,#22136),(#22137,#22138,#22139),(#22140,#22141,
#22142),(#22143,#22144,#22145),(#22146,#22147,#22148),(#22149,#22150,#22151),
(#22152,#22153,#22154),(#22155,#22156,#22157),(#22158,#22159,#22160),(#22161,
#22162,#22163),(#22164,#22165,#22166),(#22167,#22168,#22169),(#22170,#22171,
#22172),(#22173,#22174,#22175),(#22176,#22177,#22178),(#22179,#22180,#22181),
(#22182,#22183,#22184),(#22185,#22186,#22187),(#22188,#22189,#22190),(#22191,
#22192,#22193),(#22194,#22195,#22196),(#22197,#22198,#22199),(#22200,#22201,
#22202),(#22203,#22204,#22205),(#22206,#22207,#22208),(#22209,#22210,#22211),
(#22212,#22213,#22214),(#22215,#22216,#22217),(#22218,#22219,#22220),(#22221,
#22222,#22223),(#22224,#22225,#22226),(#22227,#22228,#22229),(#22230,#22231,
#22232),(#22233,#22234,#22235),(#22236,#22237,#22238),(#22239,#22240,#22241),
(#22242,#22243,#22244),(#22245,#22246,#22247),(#22248,#22249,#22250)),
 .UNSPECIFIED.,.F.,.F.,.F.)
B_SPLINE_SURFACE_WITH_KNOTS((4,2,2,2,2,2,2,2,2,2,2,2,2,2,2,2,2,2,2,2,4),
(3,3),(-1.33640092427433E-5,0.0143336398395062,0.0286672796790123,0.0430009195185185,
0.0501677394382716,0.0573345593580247,0.0716681991975309,0.086001839037037,
0.100335478876543,0.10391888883642,0.107502298796296,0.114669118716049,
0.143336398395062,0.157670038234568,0.164836858154321,0.168420268114198,
0.172003678074074,0.200670957753086,0.215004597592593,0.222171417512346,
0.229338237432099),(0.,1.00001336400924),.UNSPECIFIED.)
GEOMETRIC_REPRESENTATION_ITEM()
RATIONAL_B_SPLINE_SURFACE(((1.,0.707065702331389,1.00000782955332),(1.,
0.720365752837665,1.00000747406933),(1.,0.732997937007419,1.00000713643607),
(1.,0.757136662906848,1.00000649125576),(1.,0.768644595917913,1.00000618367152),
(1.,0.790707340875925,1.00000559397806),(1.,0.801261582208021,1.0000053118841),
(1.,0.81646072210143,1.00000490564121),(1.,0.821421417771145,1.00000477305165),
(1.,0.83114203716075,1.00000451323875),(1.,0.835878493775337,1.00000438664265),
(1.,0.849709304787154,1.00000401697248),(1.,0.858440725220516,1.00000378359891),
(1.,0.875034831571146,1.00000334007133),(1.,0.882897179367727,1.00000312992635),
(1.,0.897828694072166,1.00000273083655),(1.,0.904897666774157,1.00000254189692),
(1.,0.913269656822881,1.00000231813022),(1.,0.914920788684494,1.00000227399873),
(1.,0.918177101827732,1.00000218696394),(1.,0.919783361216391,1.0000021440318),
(1.,0.924516621769634,1.00000201752113),(1.,0.927563302847372,1.00000193608938),
(1.,0.942277686083803,1.00000154280307),(1.,0.952402217960055,1.0000012721944),
(1.,0.965415132797023,1.00000092438497),(1.,0.969387710627092,1.00000081820584),
(1.,0.97481433662669,1.00000067316288),(1.,0.976534369328306,1.00000062718981),
(1.,0.978981874496077,1.00000056177285),(1.,0.979776277220496,1.00000054054004),
(1.,0.981316478380045,1.00000049937351),(1.,0.982062500098414,1.00000047943383),
(1.,0.988563133263475,1.00000030568479),(1.,0.99283448826902,1.00000019151993),
(1.,0.99712391309534,1.0000000768721),(1.,0.998198617961198,1.00000004814737),
(1.,0.99927734527317,1.00000001931513),(1.,0.999547908598833,1.00000001208351),
(1.,0.999909373731539,1.00000000242226),(1.,1.00000013413709,0.999999999996415),
(1.,1.,1.)))
REPRESENTATION_ITEM('')
SURFACE()
);
#109=(
BOUNDED_SURFACE()
B_SPLINE_SURFACE(3,2,((#22566,#22567,#22568),(#22569,#22570,#22571),(#22572,
#22573,#22574),(#22575,#22576,#22577),(#22578,#22579,#22580),(#22581,#22582,
#22583),(#22584,#22585,#22586),(#22587,#22588,#22589),(#22590,#22591,#22592),
(#22593,#22594,#22595),(#22596,#22597,#22598),(#22599,#22600,#22601),(#22602,
#22603,#22604),(#22605,#22606,#22607),(#22608,#22609,#22610),(#22611,#22612,
#22613),(#22614,#22615,#22616),(#22617,#22618,#22619),(#22620,#22621,#22622),
(#22623,#22624,#22625)),.UNSPECIFIED.,.F.,.F.,.F.)
B_SPLINE_SURFACE_WITH_KNOTS((4,2,2,2,2,2,2,2,2,4),(3,3),(0.00505837679447142,
0.00808192097035447,0.00959369305829599,0.0111054651462375,0.012617237234179,
0.0141290093221206,0.0148848953660913,0.0156407814100621,0.0163966674540328,
0.0171525534980036),(0.,1.),.UNSPECIFIED.)
GEOMETRIC_REPRESENTATION_ITEM()
RATIONAL_B_SPLINE_SURFACE(((1.,0.707106781186547,1.),(1.,0.739053872509116,
1.),(1.,0.768433399252105,1.),(1.,0.809724042302045,1.),(1.,0.823019853650823,
1.),(1.,0.848781685567262,1.),(1.,0.861247499610797,1.),(1.,0.885026508477437,
1.),(1.,0.896438871456505,1.),(1.,0.917922922305835,1.),(1.,0.927944217122039,
1.),(1.,0.94161381312465,1.),(1.,0.945967473187117,1.),(1.,0.953895740028491,
1.),(1.,0.957485583333028,1.),(1.,0.963663001673968,1.),(1.,0.966147540420567,
1.),(1.,0.969624030438212,1.),(1.,0.970601281761249,1.),(1.,0.970581776826274,
1.)))
REPRESENTATION_ITEM('')
SURFACE()
);
#110=(
BOUNDED_SURFACE()
B_SPLINE_SURFACE(3,2,((#22864,#22865,#22866),(#22867,#22868,#22869),(#22870,
#22871,#22872),(#22873,#22874,#22875),(#22876,#22877,#22878),(#22879,#22880,
#22881),(#22882,#22883,#22884),(#22885,#22886,#22887),(#22888,#22889,#22890),
(#22891,#22892,#22893),(#22894,#22895,#22896),(#22897,#22898,#22899),(#22900,
#22901,#22902),(#22903,#22904,#22905),(#22906,#22907,#22908),(#22909,#22910,
#22911),(#22912,#22913,#22914),(#22915,#22916,#22917),(#22918,#22919,#22920),
(#22921,#22922,#22923),(#22924,#22925,#22926),(#22927,#22928,#22929)),
 .UNSPECIFIED.,.F.,.F.,.F.)
B_SPLINE_SURFACE_WITH_KNOTS((4,2,2,2,2,2,2,2,2,2,4),(3,3),(0.00605768062302923,
0.00847740131122415,0.00968726165532161,0.0108971219994191,0.0115020521714678,
0.0121069823435165,0.013316842687614,0.0139217728596627,0.0145267030317114,
0.0151316332037602,0.0157365633758089),(0.,1.),.UNSPECIFIED.)
GEOMETRIC_REPRESENTATION_ITEM()
RATIONAL_B_SPLINE_SURFACE(((1.,0.707106781186548,1.),(1.,0.678435467809058,
1.),(1.,0.648724429803459,1.),(1.,0.601883782649935,1.),(1.,0.58582572598482,
1.),(1.,0.553093074718013,1.),(1.,0.5366611790602,1.),(1.,0.512036824267513,
1.),(1.,0.503834051867292,1.),(1.,0.487490014313552,1.),(1.,0.479322252109144,
1.),(1.,0.455536119849462,1.),(1.,0.440447953764078,1.),(1.,0.420111511643565,
1.),(1.,0.413771933679107,1.),(1.,0.402532175621877,1.),(1.,0.39758573118173,
1.),(1.,0.38936895214063,1.),(1.,0.386109902300535,1.),(1.,0.381795928046837,
1.),(1.,0.380693466310634,1.),(1.,0.380693493813436,1.)))
REPRESENTATION_ITEM('')
SURFACE()
);
#111=(
BOUNDED_SURFACE()
B_SPLINE_SURFACE(3,2,((#22940,#22941,#22942),(#22943,#22944,#22945),(#22946,
#22947,#22948),(#22949,#22950,#22951),(#22952,#22953,#22954),(#22955,#22956,
#22957),(#22958,#22959,#22960),(#22961,#22962,#22963),(#22964,#22965,#22966),
(#22967,#22968,#22969),(#22970,#22971,#22972),(#22973,#22974,#22975),(#22976,
#22977,#22978),(#22979,#22980,#22981),(#22982,#22983,#22984),(#22985,#22986,
#22987),(#22988,#22989,#22990),(#22991,#22992,#22993),(#22994,#22995,#22996),
(#22997,#22998,#22999),(#23000,#23001,#23002),(#23003,#23004,#23005)),
 .UNSPECIFIED.,.F.,.F.,.F.)
B_SPLINE_SURFACE_WITH_KNOTS((4,2,2,2,2,2,2,2,2,2,4),(3,3),(0.00359639911601392,
0.00436249387044424,0.00512858862487456,0.00589468337930487,0.00666077813373519,
0.00742687288816551,0.00819296764259583,0.00972515715145646,0.0112573466603171,
0.0127895361691777,0.015853915186899),(0.,1.),.UNSPECIFIED.)
GEOMETRIC_REPRESENTATION_ITEM()
RATIONAL_B_SPLINE_SURFACE(((1.,0.970581776826274,1.),(1.,0.970578649532394,
1.),(1.,0.96964070956466,1.),(1.,0.966106916844896,1.),(1.,0.963560009136893,
1.),(1.,0.95740233193304,1.),(1.,0.953739105221087,1.),(1.,0.945797353495694,
1.),(1.,0.94149269169882,1.),(1.,0.932342624911764,1.),(1.,0.927470686999509,
1.),(1.,0.917384026303788,1.),(1.,0.912174865626315,1.),(1.,0.896095641265424,
1.),(1.,0.884778088998196,1.),(1.,0.86100319646455,1.),(1.,0.848496565440572,
1.),(1.,0.822764671287953,1.),(1.,0.809488242768719,1.),(1.,0.768270175598826,
1.),(1.,0.738957849522124,1.),(1.,0.707106781186541,1.)))
REPRESENTATION_ITEM('')
SURFACE()
);
#112=(
BOUNDED_SURFACE()
B_SPLINE_SURFACE(3,2,((#23036,#23037,#23038),(#23039,#23040,#23041),(#23042,
#23043,#23044),(#23045,#23046,#23047),(#23048,#23049,#23050),(#23051,#23052,
#23053),(#23054,#23055,#23056),(#23057,#23058,#23059),(#23060,#23061,#23062),
(#23063,#23064,#23065),(#23066,#23067,#23068),(#23069,#23070,#23071),(#23072,
#23073,#23074),(#23075,#23076,#23077),(#23078,#23079,#23080),(#23081,#23082,
#23083),(#23084,#23085,#23086),(#23087,#23088,#23089),(#23090,#23091,#23092),
(#23093,#23094,#23095)),.UNSPECIFIED.,.F.,.F.,.F.)
B_SPLINE_SURFACE_WITH_KNOTS((4,2,2,2,2,2,2,2,2,4),(3,3),(0.00387143063410007,
0.00471388371892886,0.00539035064546607,0.00606681757200329,0.0067432844985405,
0.00809621835161492,0.00944915220468934,0.0108020860577638,0.0121550199108382,
0.0150268737752786),(0.,1.00016598615829),.UNSPECIFIED.)
GEOMETRIC_REPRESENTATION_ITEM()
RATIONAL_B_SPLINE_SURFACE(((1.,0.955399887158975,1.00001480600278),(1.,
0.955829132859094,1.00001466350509),(1.,0.955152845891184,1.00001488801364),
(1.,0.952140174640701,1.0000158881371),(1.,0.95012712734567,1.00001655641307),
(1.,0.945126911092976,1.00001821634644),(1.,0.942132982861274,1.00001921024773),
(1.,0.935297780612531,1.00002147934566),(1.,0.931461499156383,1.0000227528849),
(1.,0.919200779571961,1.00002682310438),(1.,0.909918466100668,1.00002990457549),
(1.,0.889588132182854,1.00003665368354),(1.,0.878801976969414,1.00004023438847),
(1.,0.856103617498776,1.00004776961545),(1.,0.844188170450328,1.00005172521401),
(1.,0.819187865450958,1.00006002462317),(1.,0.806145836648029,1.00006435421569),
(1.,0.764361494284231,1.00007822546062),(1.,0.734139217941498,1.00008825841971),
(0.999999999999999,0.701407786598383,1.0000991243488)))
REPRESENTATION_ITEM('')
SURFACE()
);
#113=(
BOUNDED_SURFACE()
B_SPLINE_SURFACE(3,2,((#23218,#23219,#23220),(#23221,#23222,#23223),(#23224,
#23225,#23226),(#23227,#23228,#23229),(#23230,#23231,#23232),(#23233,#23234,
#23235),(#23236,#23237,#23238),(#23239,#23240,#23241),(#23242,#23243,#23244),
(#23245,#23246,#23247),(#23248,#23249,#23250),(#23251,#23252,#23253),(#23254,
#23255,#23256),(#23257,#23258,#23259),(#23260,#23261,#23262),(#23263,#23264,
#23265),(#23266,#23267,#23268),(#23269,#23270,#23271),(#23272,#23273,#23274),
(#23275,#23276,#23277)),.UNSPECIFIED.,.F.,.F.,.F.)
B_SPLINE_SURFACE_WITH_KNOTS((4,2,2,2,2,2,2,2,2,4),(3,3),(0.00433666893074964,
0.00702103924194056,0.00836322439753602,0.00970540955313147,0.0110475947087269,
0.0123897798643224,0.0130608724421201,0.0137319650199178,0.0144030575977156,
0.0150741501755133),(0.,1.),.UNSPECIFIED.)
GEOMETRIC_REPRESENTATION_ITEM()
RATIONAL_B_SPLINE_SURFACE(((1.,0.707106781186548,1.),(1.,0.737894213217654,
1.),(1.,0.766274690665779,1.),(1.,0.80619741544873,1.),(1.,0.81905917672634,
1.),(1.,0.843975019036595,1.),(1.,0.856066072681341,1.),(1.,0.878882708476932,
1.),(1.,0.889682618268665,1.),(1.,0.909952939738908,1.),(1.,0.91926443717337,
1.),(1.,0.931500456841751,1.),(1.,0.935322128839039,1.),(1.,0.942157243325948,
1.),(1.,0.945149563733463,1.),(1.,0.950144827786557,1.),(1.,0.952152129590434,
1.),(1.,0.954830461683239,1.),(1.,0.955531530247581,1.),(1.,0.95553308590591,
1.)))
REPRESENTATION_ITEM('')
SURFACE()
);
#114=(
BOUNDED_SURFACE()
B_SPLINE_SURFACE(3,2,((#23495,#23496,#23497),(#23498,#23499,#23500),(#23501,
#23502,#23503),(#23504,#23505,#23506),(#23507,#23508,#23509),(#23510,#23511,
#23512),(#23513,#23514,#23515),(#23516,#23517,#23518),(#23519,#23520,#23521),
(#23522,#23523,#23524),(#23525,#23526,#23527),(#23528,#23529,#23530),(#23531,
#23532,#23533),(#23534,#23535,#23536),(#23537,#23538,#23539),(#23540,#23541,
#23542),(#23543,#23544,#23545),(#23546,#23547,#23548),(#23549,#23550,#23551),
(#23552,#23553,#23554),(#23555,#23556,#23557),(#23558,#23559,#23560),(#23561,
#23562,#23563),(#23564,#23565,#23566)),.UNSPECIFIED.,.F.,.F.,.F.)
B_SPLINE_SURFACE_WITH_KNOTS((4,2,2,2,2,2,2,2,2,2,2,4),(3,3),(0.00449003234654763,
0.00509682357326747,0.00570361479998732,0.00631040602670716,0.00691719725342701,
0.00752398848014685,0.00813077970686669,0.00873757093358654,0.00934436216030638,
0.0105579446137461,0.0117715270671858,0.0141986919740651),(0.,1.),
 .UNSPECIFIED.)
GEOMETRIC_REPRESENTATION_ITEM()
RATIONAL_B_SPLINE_SURFACE(((1.,0.38069349381344,1.),(1.,0.380693826435357,
1.),(1.,0.381828035551871,1.),(1.,0.386153151069475,1.),(1.,0.389343566002074,
1.),(1.,0.397589118267461,1.),(1.,0.402611271260585,1.),(1.,0.413872221609166,
1.),(1.,0.420140875257451,1.),(1.,0.43367980618183,1.),(1.,0.440958379002546,
1.),(1.,0.455908840578608,1.),(1.,0.463628155372052,1.),(1.,0.479401310239419,
1.),(1.,0.487456032708626,1.),(1.,0.503805154106481,1.),(1.,0.51211354879696,
1.),(1.,0.53683753947851,1.),(1.,0.553207213585367,1.),(1.,0.585605914285066,
1.),(1.,0.601711645280215,1.),(1.,0.649056040268748,1.),(1.,0.678719733465159,
1.),(1.,0.707106781186549,1.)))
REPRESENTATION_ITEM('')
SURFACE()
);
#115=(
BOUNDED_SURFACE()
B_SPLINE_SURFACE(3,2,((#23571,#23572,#23573),(#23574,#23575,#23576),(#23577,
#23578,#23579),(#23580,#23581,#23582),(#23583,#23584,#23585),(#23586,#23587,
#23588),(#23589,#23590,#23591),(#23592,#23593,#23594),(#23595,#23596,#23597),
(#23598,#23599,#23600),(#23601,#23602,#23603),(#23604,#23605,#23606),(#23607,
#23608,#23609),(#23610,#23611,#23612),(#23613,#23614,#23615),(#23616,#23617,
#23618),(#23619,#23620,#23621),(#23622,#23623,#23624),(#23625,#23626,#23627),
(#23628,#23629,#23630)),.UNSPECIFIED.,.F.,.F.,.F.)
B_SPLINE_SURFACE_WITH_KNOTS((4,2,2,2,2,2,2,2,2,4),(3,3),(0.00505837679447142,
0.00808192097035447,0.00959369305829599,0.0111054651462375,0.012617237234179,
0.0141290093221206,0.0148848953660913,0.0156407814100621,0.0163966674540328,
0.0171525534980036),(0.,1.),.UNSPECIFIED.)
GEOMETRIC_REPRESENTATION_ITEM()
RATIONAL_B_SPLINE_SURFACE(((1.,0.707106781186547,1.),(1.,0.739053872509117,
1.),(1.,0.768433399252105,1.),(1.,0.809724042302045,1.),(1.,0.823019853650822,
1.),(1.,0.848781685567261,1.),(1.,0.861247499610797,1.),(1.,0.885026508477437,
1.),(1.,0.896438871456477,1.),(1.,0.917922922305863,1.),(1.,0.927944217122039,
1.),(1.,0.94161381312465,1.),(1.,0.945967473187117,1.),(1.,0.953895740028491,
1.),(1.,0.957485583333028,1.),(1.,0.963663001673968,1.),(1.,0.966147540420553,
1.),(1.,0.969624030438226,1.),(1.,0.970601281761238,1.),(1.,0.970581776826274,
1.)))
REPRESENTATION_ITEM('')
SURFACE()
);
#116=(
BOUNDED_SURFACE()
B_SPLINE_SURFACE(3,2,((#23752,#23753,#23754),(#23755,#23756,#23757),(#23758,
#23759,#23760),(#23761,#23762,#23763),(#23764,#23765,#23766),(#23767,#23768,
#23769),(#23770,#23771,#23772),(#23773,#23774,#23775),(#23776,#23777,#23778),
(#23779,#23780,#23781),(#23782,#23783,#23784),(#23785,#23786,#23787),(#23788,
#23789,#23790),(#23791,#23792,#23793),(#23794,#23795,#23796),(#23797,#23798,
#23799),(#23800,#23801,#23802),(#23803,#23804,#23805),(#23806,#23807,#23808),
(#23809,#23810,#23811),(#23812,#23813,#23814),(#23815,#23816,#23817)),
 .UNSPECIFIED.,.F.,.F.,.F.)
B_SPLINE_SURFACE_WITH_KNOTS((4,2,2,2,2,2,2,2,2,2,4),(3,3),(0.00359639911601392,
0.00436249387044424,0.00512858862487455,0.00589468337930487,0.00666077813373519,
0.00742687288816551,0.00819296764259582,0.00972515715145646,0.0112573466603171,
0.0127895361691777,0.015853915186899),(0.,1.),.UNSPECIFIED.)
GEOMETRIC_REPRESENTATION_ITEM()
RATIONAL_B_SPLINE_SURFACE(((1.,0.970581776826274,1.),(1.,0.970578649532459,
1.),(1.,0.969640709564574,1.),(1.,0.966106916844982,1.),(1.,0.963560009136894,
1.),(1.,0.95740233193304,1.),(1.,0.953739105221087,1.),(1.,0.945797353495694,
1.),(1.,0.94149269169882,1.),(1.,0.932342624911764,1.),(1.,0.927470686999452,
1.),(1.,0.917384026303845,1.),(1.,0.912174865626315,1.),(1.,0.896095641265424,
1.),(1.,0.884778088998393,1.),(1.,0.861003196464352,1.),(1.,0.848496565440543,
1.),(1.,0.822764671287981,1.),(1.,0.809488242768579,1.),(1.,0.768270175599105,
1.),(1.,0.738957849521914,1.),(1.,0.70710678118654,1.)))
REPRESENTATION_ITEM('')
SURFACE()
);
#117=(
BOUNDED_SURFACE()
B_SPLINE_SURFACE(3,2,((#24059,#24060,#24061),(#24062,#24063,#24064),(#24065,
#24066,#24067),(#24068,#24069,#24070),(#24071,#24072,#24073),(#24074,#24075,
#24076),(#24077,#24078,#24079),(#24080,#24081,#24082),(#24083,#24084,#24085),
(#24086,#24087,#24088),(#24089,#24090,#24091),(#24092,#24093,#24094),(#24095,
#24096,#24097),(#24098,#24099,#24100),(#24101,#24102,#24103),(#24104,#24105,
#24106),(#24107,#24108,#24109),(#24110,#24111,#24112),(#24113,#24114,#24115),
(#24116,#24117,#24118),(#24119,#24120,#24121),(#24122,#24123,#24124),(#24125,
#24126,#24127),(#24128,#24129,#24130)),.UNSPECIFIED.,.F.,.F.,.F.)
B_SPLINE_SURFACE_WITH_KNOTS((4,2,2,2,2,2,2,2,2,2,2,4),(3,3),(0.00449003234654763,
0.00509682357326747,0.00570361479998732,0.00631040602670716,0.00691719725342701,
0.00752398848014685,0.00813077970686669,0.00873757093358654,0.00934436216030638,
0.0105579446137461,0.0117715270671858,0.0141986919740651),(0.,1.),
 .UNSPECIFIED.)
GEOMETRIC_REPRESENTATION_ITEM()
RATIONAL_B_SPLINE_SURFACE(((1.,0.38069349381344,1.),(1.,0.380693826435357,
1.),(1.,0.381828035551871,1.),(1.,0.386153151069475,1.),(1.,0.389343566002074,
1.),(1.,0.397589118267461,1.),(1.,0.402611271260585,1.),(1.,0.413872221609166,
1.),(1.,0.420140875257451,1.),(1.,0.43367980618183,1.),(1.,0.440958379002546,
1.),(1.,0.455908840578608,1.),(1.,0.463628155372052,1.),(1.,0.479401310239419,
1.),(1.,0.487456032708626,1.),(1.,0.503805154106481,1.),(1.,0.51211354879696,
1.),(1.,0.53683753947851,1.),(1.,0.553207213585367,1.),(1.,0.585605914285066,
1.),(1.,0.601711645280215,1.),(1.,0.649056040268748,1.),(1.,0.678719733465158,
1.),(1.,0.707106781186549,1.)))
REPRESENTATION_ITEM('')
SURFACE()
);
#118=(
BOUNDED_SURFACE()
B_SPLINE_SURFACE(3,2,((#24136,#24137,#24138),(#24139,#24140,#24141),(#24142,
#24143,#24144),(#24145,#24146,#24147),(#24148,#24149,#24150),(#24151,#24152,
#24153),(#24154,#24155,#24156),(#24157,#24158,#24159),(#24160,#24161,#24162),
(#24163,#24164,#24165),(#24166,#24167,#24168),(#24169,#24170,#24171),(#24172,
#24173,#24174),(#24175,#24176,#24177),(#24178,#24179,#24180),(#24181,#24182,
#24183),(#24184,#24185,#24186),(#24187,#24188,#24189),(#24190,#24191,#24192),
(#24193,#24194,#24195)),.UNSPECIFIED.,.F.,.F.,.F.)
B_SPLINE_SURFACE_WITH_KNOTS((4,2,2,2,2,2,2,2,2,4),(3,3),(0.00433666893074964,
0.00702103924194056,0.00836322439753602,0.00970540955313147,0.0110475947087269,
0.0123897798643224,0.0130608724421201,0.0137319650199178,0.0144030575977156,
0.0150741501755133),(0.,1.),.UNSPECIFIED.)
GEOMETRIC_REPRESENTATION_ITEM()
RATIONAL_B_SPLINE_SURFACE(((1.,0.707106781186548,1.),(1.,0.737894213217654,
1.),(1.,0.766274690665779,1.),(1.,0.80619741544873,1.),(1.,0.81905917672634,
1.),(1.,0.843975019036595,1.),(1.,0.856066072681341,1.),(1.,0.878882708476932,
1.),(1.,0.889682618268665,1.),(1.,0.909952939738908,1.),(1.,0.91926443717337,
1.),(1.,0.931500456841751,1.),(1.,0.935322128839039,1.),(1.,0.942157243325948,
1.),(1.,0.945149563733463,1.),(1.,0.950144827786557,1.),(1.,0.952152129590434,
1.),(1.,0.954830461683239,1.),(1.,0.955531530247581,1.),(1.,0.95553308590591,
1.)))
REPRESENTATION_ITEM('')
SURFACE()
);
#119=(
BOUNDED_SURFACE()
B_SPLINE_SURFACE(3,2,((#24227,#24228,#24229),(#24230,#24231,#24232),(#24233,
#24234,#24235),(#24236,#24237,#24238),(#24239,#24240,#24241),(#24242,#24243,
#24244),(#24245,#24246,#24247),(#24248,#24249,#24250),(#24251,#24252,#24253),
(#24254,#24255,#24256),(#24257,#24258,#24259),(#24260,#24261,#24262),(#24263,
#24264,#24265),(#24266,#24267,#24268),(#24269,#24270,#24271),(#24272,#24273,
#24274),(#24275,#24276,#24277),(#24278,#24279,#24280),(#24281,#24282,#24283),
(#24284,#24285,#24286)),.UNSPECIFIED.,.F.,.F.,.F.)
B_SPLINE_SURFACE_WITH_KNOTS((4,2,2,2,2,2,2,2,2,4),(3,3),(0.0038714306340967,
0.00471388371892886,0.00539035064546608,0.00606681757200329,0.0067432844985405,
0.00809621835161492,0.00944915220468935,0.0108020860577638,0.0121550199108382,
0.015026873775282),(0.,1.00016598615829),.UNSPECIFIED.)
GEOMETRIC_REPRESENTATION_ITEM()
RATIONAL_B_SPLINE_SURFACE(((1.,0.95539988715897,1.00001480600278),(1.,0.955829132859099,
1.00001466350509),(1.,0.95515284589119,1.00001488801364),(1.,0.952140174640701,
1.0000158881371),(1.,0.95012712734567,1.00001655641307),(1.,0.945126911092976,
1.00001821634644),(1.,0.942132982861274,1.00001921024773),(1.,0.935297780612531,
1.00002147934566),(1.,0.931461499156483,1.0000227528849),(1.,0.91920077957176,
1.00002682310438),(1.,0.909918466100895,1.00002990457549),(1.,0.889588132182626,
1.00003665368354),(1.,0.878801976969414,1.00004023438847),(1.,0.856103617498775,
1.00004776961545),(1.,0.844188170450328,1.00005172521401),(1.,0.819187865450958,
1.00006002462317),(1.,0.806145836648402,1.00006435421569),(1.,0.764361494283404,
1.00007822546062),(1.,0.734139217942157,1.00008825841971),(1.,0.701407786598142,
1.0000991243488)))
REPRESENTATION_ITEM('')
SURFACE()
);
#120=(
BOUNDED_SURFACE()
B_SPLINE_SURFACE(3,2,((#24515,#24516,#24517),(#24518,#24519,#24520),(#24521,
#24522,#24523),(#24524,#24525,#24526),(#24527,#24528,#24529),(#24530,#24531,
#24532),(#24533,#24534,#24535),(#24536,#24537,#24538),(#24539,#24540,#24541),
(#24542,#24543,#24544),(#24545,#24546,#24547),(#24548,#24549,#24550),(#24551,
#24552,#24553),(#24554,#24555,#24556),(#24557,#24558,#24559),(#24560,#24561,
#24562),(#24563,#24564,#24565),(#24566,#24567,#24568),(#24569,#24570,#24571),
(#24572,#24573,#24574),(#24575,#24576,#24577),(#24578,#24579,#24580)),
 .UNSPECIFIED.,.F.,.F.,.F.)
B_SPLINE_SURFACE_WITH_KNOTS((4,2,2,2,2,2,2,2,2,2,4),(3,3),(0.00359639911601392,
0.00436249387044424,0.00512858862487455,0.00589468337930487,0.00666077813373519,
0.00742687288816551,0.00819296764259582,0.00972515715145646,0.0112573466603171,
0.0127895361691777,0.015853915186899),(0.,1.),.UNSPECIFIED.)
GEOMETRIC_REPRESENTATION_ITEM()
RATIONAL_B_SPLINE_SURFACE(((1.,0.970581776826274,1.),(1.,0.970578649532459,
1.),(1.,0.969640709564574,1.),(1.,0.966106916844982,1.),(1.,0.963560009136894,
1.),(1.,0.95740233193304,1.),(1.,0.953739105221087,1.),(1.,0.945797353495694,
1.),(1.,0.94149269169882,1.),(1.,0.932342624911764,1.),(1.,0.927470686999452,
1.),(1.,0.917384026303845,1.),(1.,0.912174865626315,1.),(1.,0.896095641265424,
1.),(1.,0.884778088998393,1.),(1.,0.861003196464352,1.),(1.,0.848496565440543,
1.),(1.,0.822764671287981,1.),(1.,0.809488242768579,1.),(1.,0.768270175599105,
1.),(1.,0.738957849521914,1.),(1.,0.70710678118654,1.)))
REPRESENTATION_ITEM('')
SURFACE()
);
#121=(
BOUNDED_SURFACE()
B_SPLINE_SURFACE(3,2,((#24584,#24585,#24586),(#24587,#24588,#24589),(#24590,
#24591,#24592),(#24593,#24594,#24595),(#24596,#24597,#24598),(#24599,#24600,
#24601),(#24602,#24603,#24604),(#24605,#24606,#24607),(#24608,#24609,#24610),
(#24611,#24612,#24613),(#24614,#24615,#24616),(#24617,#24618,#24619),(#24620,
#24621,#24622),(#24623,#24624,#24625),(#24626,#24627,#24628),(#24629,#24630,
#24631),(#24632,#24633,#24634),(#24635,#24636,#24637),(#24638,#24639,#24640),
(#24641,#24642,#24643),(#24644,#24645,#24646),(#24647,#24648,#24649)),
 .UNSPECIFIED.,.F.,.F.,.F.)
B_SPLINE_SURFACE_WITH_KNOTS((4,2,2,2,2,2,2,2,2,2,4),(3,3),(0.00605768062302923,
0.00847740131122415,0.00968726165532161,0.0108971219994191,0.0115020521714678,
0.0121069823435165,0.013316842687614,0.0139217728596627,0.0145267030317115,
0.0151316332037602,0.0157365633758089),(0.,1.),.UNSPECIFIED.)
GEOMETRIC_REPRESENTATION_ITEM()
RATIONAL_B_SPLINE_SURFACE(((1.,0.707106781186548,1.),(1.,0.678435467809629,
1.),(1.,0.6487244298027,1.),(1.,0.601883782650315,1.),(1.,0.58582572598378,
1.),(1.,0.553093074719053,1.),(1.,0.536661179059662,1.),(1.,0.512036824267783,
1.),(1.,0.503834051867293,1.),(1.,0.487490014313552,1.),(1.,0.479322252109327,
1.),(1.,0.455536119849103,1.),(1.,0.440447953764904,1.),(1.,0.420111511643149,
1.),(1.,0.413771933679518,1.),(1.,0.402532175621466,1.),(1.,0.397585731180899,
1.),(1.,0.389368952141461,1.),(1.,0.386109902300579,1.),(1.,0.38179592804679,
1.),(1.,0.380693466310667,1.),(1.,0.38069349381344,1.)))
REPRESENTATION_ITEM('')
SURFACE()
);
#122=(
BOUNDED_SURFACE()
B_SPLINE_SURFACE(3,2,((#24765,#24766,#24767),(#24768,#24769,#24770),(#24771,
#24772,#24773),(#24774,#24775,#24776),(#24777,#24778,#24779),(#24780,#24781,
#24782),(#24783,#24784,#24785),(#24786,#24787,#24788),(#24789,#24790,#24791),
(#24792,#24793,#24794),(#24795,#24796,#24797),(#24798,#24799,#24800),(#24801,
#24802,#24803),(#24804,#24805,#24806),(#24807,#24808,#24809),(#24810,#24811,
#24812),(#24813,#24814,#24815),(#24816,#24817,#24818),(#24819,#24820,#24821),
(#24822,#24823,#24824)),.UNSPECIFIED.,.F.,.F.,.F.)
B_SPLINE_SURFACE_WITH_KNOTS((4,2,2,2,2,2,2,2,2,4),(3,3),(0.00505837679447141,
0.00808192097035446,0.00959369305829598,0.0111054651462375,0.012617237234179,
0.0141290093221206,0.0148848953660913,0.0156407814100621,0.0163966674540328,
0.0171525534980036),(0.,1.),.UNSPECIFIED.)
GEOMETRIC_REPRESENTATION_ITEM()
RATIONAL_B_SPLINE_SURFACE(((1.,0.707106781186547,1.),(1.,0.739053872510172,
1.),(1.,0.768433399250703,1.),(1.,0.809724042302746,1.),(1.,0.823019853650823,
1.),(1.,0.848781685567262,1.),(1.,0.861247499610966,1.),(1.,0.885026508477268,
1.),(1.,0.896438871456985,1.),(1.,0.917922922305354,1.),(1.,0.927944217122039,
1.),(1.,0.94161381312465,1.),(1.,0.945967473187047,1.),(1.,0.953895740028562,
1.),(1.,0.957485583333028,1.),(1.,0.963663001673968,1.),(1.,0.966147540420553,
1.),(1.,0.969624030438226,1.),(1.,0.970601281761238,1.),(1.,0.970581776826274,
1.)))
REPRESENTATION_ITEM('')
SURFACE()
);
#123=(
BOUNDED_SURFACE()
B_SPLINE_SURFACE(3,2,((#24952,#24953,#24954),(#24955,#24956,#24957),(#24958,
#24959,#24960),(#24961,#24962,#24963),(#24964,#24965,#24966),(#24967,#24968,
#24969),(#24970,#24971,#24972),(#24973,#24974,#24975),(#24976,#24977,#24978),
(#24979,#24980,#24981),(#24982,#24983,#24984),(#24985,#24986,#24987),(#24988,
#24989,#24990),(#24991,#24992,#24993),(#24994,#24995,#24996),(#24997,#24998,
#24999),(#25000,#25001,#25002),(#25003,#25004,#25005),(#25006,#25007,#25008),
(#25009,#25010,#25011)),.UNSPECIFIED.,.F.,.F.,.F.)
B_SPLINE_SURFACE_WITH_KNOTS((4,2,2,2,2,2,2,2,2,4),(3,3),(0.00505837679447142,
0.00808192097035447,0.00959369305829599,0.0111054651462375,0.012617237234179,
0.0141290093221206,0.0148848953660913,0.0156407814100621,0.0163966674540328,
0.0171525534980036),(0.,1.),.UNSPECIFIED.)
GEOMETRIC_REPRESENTATION_ITEM()
RATIONAL_B_SPLINE_SURFACE(((1.,0.707106781186547,1.),(1.,0.739053872509116,
1.),(1.,0.768433399252105,1.),(1.,0.809724042302045,1.),(1.,0.823019853650823,
1.),(1.,0.848781685567262,1.),(1.,0.861247499610797,1.),(1.,0.885026508477437,
1.),(1.,0.896438871456505,1.),(1.,0.917922922305835,1.),(1.,0.927944217122039,
1.),(1.,0.94161381312465,1.),(1.,0.945967473187117,1.),(1.,0.953895740028491,
1.),(1.,0.957485583333028,1.),(1.,0.963663001673968,1.),(1.,0.966147540420567,
1.),(1.,0.969624030438212,1.),(1.,0.970601281761249,1.),(1.,0.970581776826274,
1.)))
REPRESENTATION_ITEM('')
SURFACE()
);
#124=(
BOUNDED_SURFACE()
B_SPLINE_SURFACE(3,2,((#25135,#25136,#25137),(#25138,#25139,#25140),(#25141,
#25142,#25143),(#25144,#25145,#25146),(#25147,#25148,#25149),(#25150,#25151,
#25152),(#25153,#25154,#25155),(#25156,#25157,#25158),(#25159,#25160,#25161),
(#25162,#25163,#25164),(#25165,#25166,#25167),(#25168,#25169,#25170),(#25171,
#25172,#25173),(#25174,#25175,#25176),(#25177,#25178,#25179),(#25180,#25181,
#25182),(#25183,#25184,#25185),(#25186,#25187,#25188),(#25189,#25190,#25191),
(#25192,#25193,#25194),(#25195,#25196,#25197),(#25198,#25199,#25200)),
 .UNSPECIFIED.,.F.,.F.,.F.)
B_SPLINE_SURFACE_WITH_KNOTS((4,2,2,2,2,2,2,2,2,2,4),(3,3),(0.00359639911601392,
0.00436249387044424,0.00512858862487455,0.00589468337930487,0.00666077813373519,
0.00742687288816551,0.00819296764259582,0.00972515715145646,0.0112573466603171,
0.0127895361691777,0.015853915186899),(0.,1.),.UNSPECIFIED.)
GEOMETRIC_REPRESENTATION_ITEM()
RATIONAL_B_SPLINE_SURFACE(((1.,0.970581776826274,1.),(1.,0.970578649532459,
1.),(1.,0.969640709564574,1.),(1.,0.966106916844982,1.),(1.,0.963560009136894,
1.),(1.,0.95740233193304,1.),(1.,0.953739105221087,1.),(1.,0.945797353495694,
1.),(1.,0.94149269169882,1.),(1.,0.932342624911764,1.),(1.,0.927470686999466,
1.),(1.,0.917384026303831,1.),(1.,0.912174865626315,1.),(1.,0.896095641265424,
1.),(1.,0.884778088998309,1.),(1.,0.861003196464437,1.),(1.,0.848496565440628,
1.),(1.,0.822764671287897,1.),(1.,0.809488242768719,1.),(1.,0.768270175598826,
1.),(1.,0.738957849522124,1.),(1.,0.70710678118654,1.)))
REPRESENTATION_ITEM('')
SURFACE()
);
#125=ELLIPSE('',#12050,36.0279058508802,34.9999999999993);
#126=ELLIPSE('',#12051,36.0279058508828,35.0000000000005);
#127=ELLIPSE('',#12052,35.3413355718209,35.0000000000005);
#128=ELLIPSE('',#12053,35.34133557182,34.9999999999995);
#129=ELLIPSE('',#12054,25.2438111227311,25.0000000000022);
#130=ELLIPSE('',#12055,25.24381112273,25.0000000000009);
#131=ELLIPSE('',#12056,25.7342184649135,24.9999999999991);
#132=ELLIPSE('',#12057,25.7342184649167,25.0000000000005);
#133=ELLIPSE('',#12698,2.59172390171958,2.54000000000056);
#134=ELLIPSE('',#12701,6.9976545346413,6.85800000000022);
#135=ELLIPSE('',#12704,6.99765453464393,6.85800000000241);
#136=ELLIPSE('',#12707,2.59172390171943,2.54000000000021);
#137=ELLIPSE('',#12712,2.59172390172017,2.54000000000112);
#138=ELLIPSE('',#12713,6.99765453464255,6.8580000000014);
#139=ELLIPSE('',#12714,6.99765453464257,6.85800000000131);
#140=ELLIPSE('',#12715,2.59172390172489,2.5400000000054);
#141=ELLIPSE('',#12720,2.59172390172243,2.54000000000345);
#142=ELLIPSE('',#12723,6.99765453464225,6.85800000000097);
#143=ELLIPSE('',#12726,6.99765453464551,6.8580000000038);
#144=ELLIPSE('',#12729,2.59172390171343,2.53999999999498);
#145=ELLIPSE('',#12737,2.59172390171873,2.53999999999979);
#146=ELLIPSE('',#12741,6.99765453464068,6.85799999999964);
#147=ELLIPSE('',#12745,6.99765453464442,6.85800000000265);
#148=ELLIPSE('',#12749,2.5917239017157,2.53999999999687);
#149=ELLIPSE('',#12786,2.59172390172123,2.54000000000197);
#150=ELLIPSE('',#12789,6.99765453463971,6.85799999999854);
#151=ELLIPSE('',#12792,6.99765453464465,6.85800000000273);
#152=ELLIPSE('',#12795,2.59172390171767,2.53999999999863);
#153=ELLIPSE('',#12802,2.59172390172269,2.54000000000292);
#154=ELLIPSE('',#12806,6.99765453464155,6.85800000000042);
#155=ELLIPSE('',#12810,6.99765453463736,6.85799999999707);
#156=ELLIPSE('',#12814,2.59172390171622,2.5399999999978);
#157=ELLIPSE('',#12822,2.59172390171995,2.54000000000139);
#158=ELLIPSE('',#12823,6.99765453464566,6.85800000000388);
#159=ELLIPSE('',#12824,6.99765453464157,6.85800000000006);
#160=ELLIPSE('',#12825,2.59172390171781,2.53999999999902);
#161=ELLIPSE('',#12830,2.59172390171478,2.53999999999635);
#162=ELLIPSE('',#12833,6.99765453464405,6.85800000000235);
#163=ELLIPSE('',#12836,6.99765453464219,6.85800000000072);
#164=ELLIPSE('',#12839,2.59172390171126,2.53999999999298);
#165=ELLIPSE('',#12852,3.59210244842959,2.54000000000127);
#166=ELLIPSE('',#12855,9.69867661075609,6.8580000000008);
#167=ELLIPSE('',#12858,9.69867661075375,6.85799999999966);
#168=ELLIPSE('',#12861,3.59210244842762,2.54000000000046);
#169=ELLIPSE('',#12874,3.59210244842275,2.53999999999717);
#170=ELLIPSE('',#12877,9.69867661074225,6.8579999999926);
#171=ELLIPSE('',#12880,9.69867661075566,6.85800000000089);
#172=ELLIPSE('',#12883,3.59210244842444,2.53999999999849);
#173=ELLIPSE('',#12962,4.48294385563966,3.16992000000064);
#174=ELLIPSE('',#12965,6.73519209081142,4.76250000000638);
#175=ELLIPSE('',#12968,4.48294385563524,3.16991999999855);
#176=ELLIPSE('',#12975,4.48294385564325,3.16992000000392);
#177=ELLIPSE('',#12976,4.48294385563259,3.16991999999665);
#178=ELLIPSE('',#12979,6.73519209080091,4.76249999999985);
#179=ELLIPSE('',#12980,6.735192090809,4.76250000000462);
#180=ELLIPSE('',#12983,4.48294385564188,3.16992000000291);
#181=ELLIPSE('',#12984,4.48294385563158,3.16991999999587);
#182=ELLIPSE('',#12996,4.48294385563683,3.16991999999945);
#183=ELLIPSE('',#12999,6.73519209079765,4.7624999999967);
#184=ELLIPSE('',#13002,4.48294385564503,3.16992000000453);
#185=ELLIPSE('',#13013,4.482943855623,3.16991999998934);
#186=ELLIPSE('',#13016,6.73519209079788,4.76249999999742);
#187=ELLIPSE('',#13019,4.48294385563564,3.16991999999873);
#188=ELLIPSE('',#13026,4.48294385563249,3.16991999999556);
#189=ELLIPSE('',#13027,4.48294385564679,3.16992000000566);
#190=ELLIPSE('',#13030,6.73519209079125,4.76249999999378);
#191=ELLIPSE('',#13031,6.73519209079818,4.76249999999747);
#192=ELLIPSE('',#13034,4.48294385563025,3.16991999999552);
#193=ELLIPSE('',#13035,4.48294385563672,3.16991999999823);
#194=ELLIPSE('',#13047,4.48294385564801,3.16992000000646);
#195=ELLIPSE('',#13050,6.73519209080312,4.76250000000048);
#196=ELLIPSE('',#13053,4.48294385563554,3.16991999999886);
#197=ELLIPSE('',#13108,3.59210244842469,2.53999999999847);
#198=ELLIPSE('',#13109,3.59210244843125,2.54000000000209);
#199=ELLIPSE('',#13112,9.69867661075553,6.85800000000037);
#200=ELLIPSE('',#13113,9.69867661075507,6.85800000000035);
#201=ELLIPSE('',#13116,9.69867661075306,6.85799999999952);
#202=ELLIPSE('',#13117,9.6986766107561,6.85800000000094);
#203=ELLIPSE('',#13120,3.592102448417,2.53999999999353);
#204=ELLIPSE('',#13121,3.59210244843681,2.54000000000594);
#205=PLANE('',#12019);
#206=PLANE('',#12020);
#207=PLANE('',#12025);
#208=PLANE('',#12030);
#209=PLANE('',#12034);
#210=PLANE('',#12044);
#211=PLANE('',#12049);
#212=PLANE('',#12058);
#213=PLANE('',#12061);
#214=PLANE('',#12063);
#215=PLANE('',#12065);
#216=PLANE('',#12109);
#217=PLANE('',#12114);
#218=PLANE('',#12124);
#219=PLANE('',#12129);
#220=PLANE('',#12132);
#221=PLANE('',#12134);
#222=PLANE('',#12136);
#223=PLANE('',#12180);
#224=PLANE('',#12181);
#225=PLANE('',#12182);
#226=PLANE('',#12184);
#227=PLANE('',#12186);
#228=PLANE('',#12187);
#229=PLANE('',#12189);
#230=PLANE('',#12191);
#231=PLANE('',#12192);
#232=PLANE('',#12194);
#233=PLANE('',#12196);
#234=PLANE('',#12197);
#235=PLANE('',#12199);
#236=PLANE('',#12201);
#237=PLANE('',#12202);
#238=PLANE('',#12204);
#239=PLANE('',#12206);
#240=PLANE('',#12207);
#241=PLANE('',#12209);
#242=PLANE('',#12211);
#243=PLANE('',#12212);
#244=PLANE('',#12213);
#245=PLANE('',#12214);
#246=PLANE('',#12215);
#247=PLANE('',#12216);
#248=PLANE('',#12491);
#249=PLANE('',#12492);
#250=PLANE('',#12493);
#251=PLANE('',#12494);
#252=PLANE('',#12495);
#253=PLANE('',#12496);
#254=PLANE('',#12497);
#255=PLANE('',#12498);
#256=PLANE('',#12499);
#257=PLANE('',#12500);
#258=PLANE('',#12501);
#259=PLANE('',#12512);
#260=PLANE('',#12513);
#261=PLANE('',#12514);
#262=PLANE('',#12515);
#263=PLANE('',#12516);
#264=PLANE('',#12520);
#265=PLANE('',#12521);
#266=PLANE('',#12524);
#267=PLANE('',#12525);
#268=PLANE('',#12529);
#269=PLANE('',#12530);
#270=PLANE('',#12532);
#271=PLANE('',#12533);
#272=PLANE('',#12537);
#273=PLANE('',#12538);
#274=PLANE('',#12540);
#275=PLANE('',#12541);
#276=PLANE('',#12545);
#277=PLANE('',#12546);
#278=PLANE('',#12548);
#279=PLANE('',#12549);
#280=PLANE('',#12553);
#281=PLANE('',#12554);
#282=PLANE('',#12556);
#283=PLANE('',#12557);
#284=PLANE('',#12561);
#285=PLANE('',#12562);
#286=PLANE('',#12564);
#287=PLANE('',#12565);
#288=PLANE('',#12569);
#289=PLANE('',#12570);
#290=PLANE('',#12572);
#291=PLANE('',#12573);
#292=PLANE('',#12577);
#293=PLANE('',#12578);
#294=PLANE('',#12580);
#295=PLANE('',#12581);
#296=PLANE('',#12585);
#297=PLANE('',#12586);
#298=PLANE('',#12588);
#299=PLANE('',#12589);
#300=PLANE('',#12593);
#301=PLANE('',#12594);
#302=PLANE('',#12605);
#303=PLANE('',#12606);
#304=PLANE('',#12607);
#305=PLANE('',#12608);
#306=PLANE('',#12609);
#307=PLANE('',#12610);
#308=PLANE('',#12611);
#309=PLANE('',#12612);
#310=PLANE('',#12613);
#311=PLANE('',#12614);
#312=PLANE('',#12615);
#313=PLANE('',#12616);
#314=PLANE('',#12617);
#315=PLANE('',#12618);
#316=PLANE('',#12664);
#317=PLANE('',#12665);
#318=PLANE('',#12667);
#319=PLANE('',#12668);
#320=PLANE('',#12672);
#321=PLANE('',#12676);
#322=PLANE('',#12680);
#323=PLANE('',#12684);
#324=PLANE('',#12685);
#325=PLANE('',#12686);
#326=PLANE('',#12687);
#327=PLANE('',#12688);
#328=PLANE('',#12689);
#329=PLANE('',#12694);
#330=PLANE('',#12695);
#331=PLANE('',#12696);
#332=PLANE('',#12699);
#333=PLANE('',#12702);
#334=PLANE('',#12705);
#335=PLANE('',#12708);
#336=PLANE('',#12709);
#337=PLANE('',#12710);
#338=PLANE('',#12711);
#339=PLANE('',#12716);
#340=PLANE('',#12717);
#341=PLANE('',#12718);
#342=PLANE('',#12721);
#343=PLANE('',#12724);
#344=PLANE('',#12727);
#345=PLANE('',#12730);
#346=PLANE('',#12731);
#347=PLANE('',#12732);
#348=PLANE('',#12733);
#349=PLANE('',#12734);
#350=PLANE('',#12738);
#351=PLANE('',#12742);
#352=PLANE('',#12746);
#353=PLANE('',#12750);
#354=PLANE('',#12751);
#355=PLANE('',#12752);
#356=PLANE('',#12753);
#357=PLANE('',#12754);
#358=PLANE('',#12755);
#359=PLANE('',#12756);
#360=PLANE('',#12760);
#361=PLANE('',#12764);
#362=PLANE('',#12768);
#363=PLANE('',#12772);
#364=PLANE('',#12773);
#365=PLANE('',#12774);
#366=PLANE('',#12775);
#367=PLANE('',#12776);
#368=PLANE('',#12777);
#369=PLANE('',#12782);
#370=PLANE('',#12783);
#371=PLANE('',#12784);
#372=PLANE('',#12787);
#373=PLANE('',#12790);
#374=PLANE('',#12793);
#375=PLANE('',#12796);
#376=PLANE('',#12797);
#377=PLANE('',#12798);
#378=PLANE('',#12799);
#379=PLANE('',#12800);
#380=PLANE('',#12804);
#381=PLANE('',#12808);
#382=PLANE('',#12812);
#383=PLANE('',#12816);
#384=PLANE('',#12817);
#385=PLANE('',#12818);
#386=PLANE('',#12819);
#387=PLANE('',#12820);
#388=PLANE('',#12821);
#389=PLANE('',#12826);
#390=PLANE('',#12827);
#391=PLANE('',#12828);
#392=PLANE('',#12831);
#393=PLANE('',#12834);
#394=PLANE('',#12837);
#395=PLANE('',#12840);
#396=PLANE('',#12841);
#397=PLANE('',#12842);
#398=PLANE('',#12843);
#399=PLANE('',#12848);
#400=PLANE('',#12849);
#401=PLANE('',#12850);
#402=PLANE('',#12853);
#403=PLANE('',#12856);
#404=PLANE('',#12859);
#405=PLANE('',#12862);
#406=PLANE('',#12863);
#407=PLANE('',#12864);
#408=PLANE('',#12865);
#409=PLANE('',#12870);
#410=PLANE('',#12871);
#411=PLANE('',#12872);
#412=PLANE('',#12875);
#413=PLANE('',#12878);
#414=PLANE('',#12881);
#415=PLANE('',#12884);
#416=PLANE('',#12885);
#417=PLANE('',#12886);
#418=PLANE('',#12887);
#419=PLANE('',#12888);
#420=PLANE('',#12892);
#421=PLANE('',#12896);
#422=PLANE('',#12900);
#423=PLANE('',#12901);
#424=PLANE('',#12902);
#425=PLANE('',#12903);
#426=PLANE('',#12904);
#427=PLANE('',#12905);
#428=PLANE('',#12909);
#429=PLANE('',#12913);
#430=PLANE('',#12917);
#431=PLANE('',#12918);
#432=PLANE('',#12919);
#433=PLANE('',#12920);
#434=PLANE('',#12921);
#435=PLANE('',#12922);
#436=PLANE('',#12926);
#437=PLANE('',#12930);
#438=PLANE('',#12934);
#439=PLANE('',#12935);
#440=PLANE('',#12936);
#441=PLANE('',#12937);
#442=PLANE('',#12938);
#443=PLANE('',#12939);
#444=PLANE('',#12943);
#445=PLANE('',#12947);
#446=PLANE('',#12951);
#447=PLANE('',#12952);
#448=PLANE('',#12953);
#449=PLANE('',#12954);
#450=PLANE('',#12955);
#451=PLANE('',#12959);
#452=PLANE('',#12960);
#453=PLANE('',#12963);
#454=PLANE('',#12966);
#455=PLANE('',#12969);
#456=PLANE('',#12970);
#457=PLANE('',#12971);
#458=PLANE('',#12972);
#459=PLANE('',#12973);
#460=PLANE('',#12977);
#461=PLANE('',#12981);
#462=PLANE('',#12985);
#463=PLANE('',#12986);
#464=PLANE('',#12987);
#465=PLANE('',#12988);
#466=PLANE('',#12989);
#467=PLANE('',#12993);
#468=PLANE('',#12994);
#469=PLANE('',#12997);
#470=PLANE('',#13000);
#471=PLANE('',#13003);
#472=PLANE('',#13004);
#473=PLANE('',#13005);
#474=PLANE('',#13006);
#475=PLANE('',#13010);
#476=PLANE('',#13011);
#477=PLANE('',#13014);
#478=PLANE('',#13017);
#479=PLANE('',#13020);
#480=PLANE('',#13021);
#481=PLANE('',#13022);
#482=PLANE('',#13023);
#483=PLANE('',#13024);
#484=PLANE('',#13028);
#485=PLANE('',#13032);
#486=PLANE('',#13036);
#487=PLANE('',#13037);
#488=PLANE('',#13038);
#489=PLANE('',#13039);
#490=PLANE('',#13040);
#491=PLANE('',#13044);
#492=PLANE('',#13045);
#493=PLANE('',#13048);
#494=PLANE('',#13051);
#495=PLANE('',#13054);
#496=PLANE('',#13055);
#497=PLANE('',#13056);
#498=PLANE('',#13069);
#499=PLANE('',#13070);
#500=PLANE('',#13071);
#501=PLANE('',#13072);
#502=PLANE('',#13073);
#503=PLANE('',#13078);
#504=PLANE('',#13083);
#505=PLANE('',#13085);
#506=PLANE('',#13086);
#507=PLANE('',#13088);
#508=PLANE('',#13089);
#509=PLANE('',#13091);
#510=PLANE('',#13092);
#511=PLANE('',#13094);
#512=PLANE('',#13095);
#513=PLANE('',#13096);
#514=PLANE('',#13097);
#515=PLANE('',#13098);
#516=PLANE('',#13105);
#517=PLANE('',#13106);
#518=PLANE('',#13110);
#519=PLANE('',#13114);
#520=PLANE('',#13118);
#521=PLANE('',#13122);
#522=PLANE('',#13123);
#523=PLANE('',#13124);
#524=PLANE('',#13125);
#525=PLANE('',#13126);
#526=PLANE('',#13133);
#527=PLANE('',#13134);
#528=PLANE('',#13138);
#529=PLANE('',#13142);
#530=PLANE('',#13146);
#531=PLANE('',#13147);
#532=PLANE('',#13148);
#533=PLANE('',#13149);
#534=PLANE('',#13156);
#535=PLANE('',#13157);
#536=PLANE('',#13161);
#537=PLANE('',#13165);
#538=PLANE('',#13169);
#539=PLANE('',#13170);
#540=PLANE('',#13171);
#541=PLANE('',#13172);
#542=FACE_BOUND('',#1419,.T.);
#543=FACE_BOUND('',#1420,.T.);
#544=FACE_BOUND('',#1422,.T.);
#545=FACE_BOUND('',#1423,.T.);
#546=FACE_BOUND('',#1425,.T.);
#547=FACE_BOUND('',#1426,.T.);
#548=FACE_BOUND('',#1428,.T.);
#549=FACE_BOUND('',#1429,.T.);
#550=FACE_BOUND('',#1431,.T.);
#551=FACE_BOUND('',#1437,.T.);
#552=FACE_BOUND('',#1470,.T.);
#553=FACE_BOUND('',#1508,.T.);
#554=FACE_BOUND('',#1509,.T.);
#555=FACE_BOUND('',#1532,.T.);
#556=FACE_BOUND('',#1533,.T.);
#557=FACE_BOUND('',#1534,.T.);
#558=FACE_BOUND('',#1535,.T.);
#559=FACE_BOUND('',#1536,.T.);
#560=FACE_BOUND('',#1537,.T.);
#561=FACE_BOUND('',#1538,.T.);
#562=FACE_BOUND('',#1540,.T.);
#563=FACE_BOUND('',#1541,.T.);
#564=FACE_BOUND('',#1542,.T.);
#565=FACE_BOUND('',#1543,.T.);
#566=FACE_BOUND('',#1544,.T.);
#567=FACE_BOUND('',#1545,.T.);
#568=FACE_BOUND('',#1546,.T.);
#569=FACE_BOUND('',#1666,.T.);
#570=FACE_BOUND('',#1667,.T.);
#571=FACE_BOUND('',#1668,.T.);
#572=FACE_BOUND('',#1669,.T.);
#573=FACE_BOUND('',#1670,.T.);
#574=FACE_BOUND('',#1671,.T.);
#575=FACE_BOUND('',#1672,.T.);
#576=FACE_BOUND('',#1673,.T.);
#577=FACE_BOUND('',#1674,.T.);
#578=FACE_BOUND('',#1688,.T.);
#579=FACE_BOUND('',#1690,.T.);
#580=FACE_BOUND('',#1692,.T.);
#581=FACE_BOUND('',#1694,.T.);
#582=FACE_BOUND('',#1766,.T.);
#583=FACE_BOUND('',#1787,.T.);
#584=FACE_BOUND('',#1788,.T.);
#585=FACE_BOUND('',#1789,.T.);
#586=FACE_BOUND('',#1790,.T.);
#587=FACE_BOUND('',#1791,.T.);
#588=FACE_BOUND('',#1792,.T.);
#589=FACE_BOUND('',#1793,.T.);
#590=FACE_BOUND('',#1795,.T.);
#591=FACE_BOUND('',#1796,.T.);
#592=FACE_BOUND('',#1797,.T.);
#593=FACE_BOUND('',#1798,.T.);
#594=FACE_BOUND('',#1799,.T.);
#595=FACE_BOUND('',#1800,.T.);
#596=FACE_BOUND('',#1801,.T.);
#597=FACE_BOUND('',#2061,.T.);
#598=FACE_BOUND('',#2062,.T.);
#599=FACE_BOUND('',#2063,.T.);
#600=FACE_BOUND('',#2064,.T.);
#601=FACE_BOUND('',#2066,.T.);
#602=FACE_BOUND('',#2067,.T.);
#603=FACE_BOUND('',#2068,.T.);
#604=FACE_BOUND('',#2069,.T.);
#605=FACE_BOUND('',#2094,.T.);
#606=FACE_BOUND('',#2095,.T.);
#607=FACE_BOUND('',#2102,.T.);
#608=FACE_BOUND('',#2103,.T.);
#609=FACE_BOUND('',#2109,.T.);
#610=FACE_BOUND('',#2110,.T.);
#611=FACE_BOUND('',#2114,.T.);
#612=FACE_BOUND('',#2115,.T.);
#613=FACE_BOUND('',#2126,.T.);
#614=FACE_BOUND('',#2127,.T.);
#615=FACE_BOUND('',#2131,.T.);
#616=FACE_BOUND('',#2132,.T.);
#617=CONICAL_SURFACE('',#11940,5.025,0.785398163397475);
#618=CONICAL_SURFACE('',#11945,5.025,0.785398163397475);
#619=CONICAL_SURFACE('',#11950,5.025,0.785398163397463);
#620=CONICAL_SURFACE('',#11955,5.025,0.785398163397475);
#621=CONICAL_SURFACE('',#11960,5.025,0.785398163397475);
#622=CONICAL_SURFACE('',#11965,5.025,0.785398163397463);
#623=CONICAL_SURFACE('',#11971,35.5,0.785398163397469);
#624=CONICAL_SURFACE('',#11974,35.5,0.785398163397469);
#625=CONICAL_SURFACE('',#12425,37.0000000000001,0.78539816339744);
#626=CONICAL_SURFACE('',#12429,30.,0.785398163397422);
#627=CONICAL_SURFACE('',#12433,35.,0.785398163397445);
#628=CONICAL_SURFACE('',#12630,6.00000000000001,0.785398163397452);
#629=CONICAL_SURFACE('',#12635,6.00000000000001,0.785398163397452);
#630=CONICAL_SURFACE('',#12640,6.,0.785398163397453);
#631=CONICAL_SURFACE('',#12645,6.00000000000001,0.785398163397452);
#632=CONICAL_SURFACE('',#12650,6.00000000000001,0.785398163397452);
#633=CONICAL_SURFACE('',#12655,6.,0.785398163397453);
#634=SPHERICAL_SURFACE('',#11914,2.5);
#635=SPHERICAL_SURFACE('',#11918,2.5);
#636=SPHERICAL_SURFACE('',#11922,2.5);
#637=SPHERICAL_SURFACE('',#11926,2.5);
#638=SPHERICAL_SURFACE('',#12223,2.5);
#639=SPHERICAL_SURFACE('',#12227,2.5);
#640=SPHERICAL_SURFACE('',#12254,2.5);
#641=SPHERICAL_SURFACE('',#12256,2.5);
#642=SPHERICAL_SURFACE('',#12259,2.5);
#643=SPHERICAL_SURFACE('',#12276,2.5);
#644=SPHERICAL_SURFACE('',#12279,2.5);
#645=SPHERICAL_SURFACE('',#12292,2.5);
#646=SPHERICAL_SURFACE('',#12317,2.5);
#647=SPHERICAL_SURFACE('',#12333,2.5);
#648=SPHERICAL_SURFACE('',#12335,2.5);
#649=SPHERICAL_SURFACE('',#12337,2.5);
#650=SPHERICAL_SURFACE('',#12340,2.5);
#651=SPHERICAL_SURFACE('',#12353,2.5);
#652=SPHERICAL_SURFACE('',#12355,2.5);
#653=SPHERICAL_SURFACE('',#12366,2.5);
#654=SPHERICAL_SURFACE('',#12369,2.5);
#655=SPHERICAL_SURFACE('',#12399,2.5);
#656=SPHERICAL_SURFACE('',#12410,2.5);
#657=SPHERICAL_SURFACE('',#12420,2.5);
#658=TOROIDAL_SURFACE('',#11899,167.5,2.5);
#659=TOROIDAL_SURFACE('',#11930,194.,1.);
#660=TOROIDAL_SURFACE('',#11935,194.,1.);
#661=TOROIDAL_SURFACE('',#12081,135.,35.);
#662=TOROIDAL_SURFACE('',#12083,210.,35.);
#663=TOROIDAL_SURFACE('',#12088,135.,35.);
#664=TOROIDAL_SURFACE('',#12090,210.,35.);
#665=TOROIDAL_SURFACE('',#12093,135.,35.);
#666=TOROIDAL_SURFACE('',#12096,250.,35.);
#667=TOROIDAL_SURFACE('',#12099,135.,35.);
#668=TOROIDAL_SURFACE('',#12102,250.,35.);
#669=TOROIDAL_SURFACE('',#12104,185.,15.);
#670=TOROIDAL_SURFACE('',#12107,185.,15.);
#671=TOROIDAL_SURFACE('',#12152,135.,25.);
#672=TOROIDAL_SURFACE('',#12154,210.,25.);
#673=TOROIDAL_SURFACE('',#12159,135.,25.);
#674=TOROIDAL_SURFACE('',#12161,210.,25.);
#675=TOROIDAL_SURFACE('',#12164,135.,25.);
#676=TOROIDAL_SURFACE('',#12167,250.,25.);
#677=TOROIDAL_SURFACE('',#12170,135.,25.);
#678=TOROIDAL_SURFACE('',#12173,250.,25.);
#679=TOROIDAL_SURFACE('',#12175,185.,25.);
#680=TOROIDAL_SURFACE('',#12178,185.,25.);
#681=TOROIDAL_SURFACE('',#12221,172.5,2.5);
#682=TOROIDAL_SURFACE('',#12231,5.,2.5);
#683=TOROIDAL_SURFACE('',#12261,5.,2.5);
#684=TOROIDAL_SURFACE('',#12264,172.5,2.5);
#685=TOROIDAL_SURFACE('',#12274,172.5,2.5);
#686=TOROIDAL_SURFACE('',#12294,5.,2.5);
#687=TOROIDAL_SURFACE('',#12297,172.5,2.5);
#688=TOROIDAL_SURFACE('',#12303,172.5,2.5);
#689=TOROIDAL_SURFACE('',#12306,5.,2.5);
#690=TOROIDAL_SURFACE('',#12316,172.5,2.5);
#691=TOROIDAL_SURFACE('',#12350,172.5,2.5);
#692=TOROIDAL_SURFACE('',#12372,172.5,2.5);
#693=TOROIDAL_SURFACE('',#12379,172.5,2.5);
#694=TOROIDAL_SURFACE('',#12382,5.,2.5);
#695=TOROIDAL_SURFACE('',#12394,5.,2.5);
#696=TOROIDAL_SURFACE('',#12396,5.,2.5);
#697=TOROIDAL_SURFACE('',#12401,172.5,2.5);
#698=TOROIDAL_SURFACE('',#12408,172.5,2.5);
#699=TOROIDAL_SURFACE('',#12411,5.,2.5);
#700=TOROIDAL_SURFACE('',#12423,172.5,2.5);
#701=TOROIDAL_SURFACE('',#12620,194.,1.);
#702=TOROIDAL_SURFACE('',#12625,194.,1.);
#703=FACE_OUTER_BOUND('',#1384,.T.);
#704=FACE_OUTER_BOUND('',#1385,.T.);
#705=FACE_OUTER_BOUND('',#1386,.T.);
#706=FACE_OUTER_BOUND('',#1387,.T.);
#707=FACE_OUTER_BOUND('',#1388,.T.);
#708=FACE_OUTER_BOUND('',#1389,.T.);
#709=FACE_OUTER_BOUND('',#1390,.T.);
#710=FACE_OUTER_BOUND('',#1391,.T.);
#711=FACE_OUTER_BOUND('',#1392,.T.);
#712=FACE_OUTER_BOUND('',#1393,.T.);
#713=FACE_OUTER_BOUND('',#1394,.T.);
#714=FACE_OUTER_BOUND('',#1395,.T.);
#715=FACE_OUTER_BOUND('',#1396,.T.);
#716=FACE_OUTER_BOUND('',#1397,.T.);
#717=FACE_OUTER_BOUND('',#1398,.T.);
#718=FACE_OUTER_BOUND('',#1399,.T.);
#719=FACE_OUTER_BOUND('',#1400,.T.);
#720=FACE_OUTER_BOUND('',#1401,.T.);
#721=FACE_OUTER_BOUND('',#1402,.T.);
#722=FACE_OUTER_BOUND('',#1403,.T.);
#723=FACE_OUTER_BOUND('',#1404,.T.);
#724=FACE_OUTER_BOUND('',#1405,.T.);
#725=FACE_OUTER_BOUND('',#1406,.T.);
#726=FACE_OUTER_BOUND('',#1407,.T.);
#727=FACE_OUTER_BOUND('',#1408,.T.);
#728=FACE_OUTER_BOUND('',#1409,.T.);
#729=FACE_OUTER_BOUND('',#1410,.T.);
#730=FACE_OUTER_BOUND('',#1411,.T.);
#731=FACE_OUTER_BOUND('',#1412,.T.);
#732=FACE_OUTER_BOUND('',#1413,.T.);
#733=FACE_OUTER_BOUND('',#1414,.T.);
#734=FACE_OUTER_BOUND('',#1415,.T.);
#735=FACE_OUTER_BOUND('',#1416,.T.);
#736=FACE_OUTER_BOUND('',#1417,.T.);
#737=FACE_OUTER_BOUND('',#1418,.T.);
#738=FACE_OUTER_BOUND('',#1421,.T.);
#739=FACE_OUTER_BOUND('',#1424,.T.);
#740=FACE_OUTER_BOUND('',#1427,.T.);
#741=FACE_OUTER_BOUND('',#1430,.T.);
#742=FACE_OUTER_BOUND('',#1432,.T.);
#743=FACE_OUTER_BOUND('',#1433,.T.);
#744=FACE_OUTER_BOUND('',#1434,.T.);
#745=FACE_OUTER_BOUND('',#1435,.T.);
#746=FACE_OUTER_BOUND('',#1436,.T.);
#747=FACE_OUTER_BOUND('',#1438,.T.);
#748=FACE_OUTER_BOUND('',#1439,.T.);
#749=FACE_OUTER_BOUND('',#1440,.T.);
#750=FACE_OUTER_BOUND('',#1441,.T.);
#751=FACE_OUTER_BOUND('',#1442,.T.);
#752=FACE_OUTER_BOUND('',#1443,.T.);
#753=FACE_OUTER_BOUND('',#1444,.T.);
#754=FACE_OUTER_BOUND('',#1445,.T.);
#755=FACE_OUTER_BOUND('',#1446,.T.);
#756=FACE_OUTER_BOUND('',#1447,.T.);
#757=FACE_OUTER_BOUND('',#1448,.T.);
#758=FACE_OUTER_BOUND('',#1449,.T.);
#759=FACE_OUTER_BOUND('',#1450,.T.);
#760=FACE_OUTER_BOUND('',#1451,.T.);
#761=FACE_OUTER_BOUND('',#1452,.T.);
#762=FACE_OUTER_BOUND('',#1453,.T.);
#763=FACE_OUTER_BOUND('',#1454,.T.);
#764=FACE_OUTER_BOUND('',#1455,.T.);
#765=FACE_OUTER_BOUND('',#1456,.T.);
#766=FACE_OUTER_BOUND('',#1457,.T.);
#767=FACE_OUTER_BOUND('',#1458,.T.);
#768=FACE_OUTER_BOUND('',#1459,.T.);
#769=FACE_OUTER_BOUND('',#1460,.T.);
#770=FACE_OUTER_BOUND('',#1461,.T.);
#771=FACE_OUTER_BOUND('',#1462,.T.);
#772=FACE_OUTER_BOUND('',#1463,.T.);
#773=FACE_OUTER_BOUND('',#1464,.T.);
#774=FACE_OUTER_BOUND('',#1465,.T.);
#775=FACE_OUTER_BOUND('',#1466,.T.);
#776=FACE_OUTER_BOUND('',#1467,.T.);
#777=FACE_OUTER_BOUND('',#1468,.T.);
#778=FACE_OUTER_BOUND('',#1469,.T.);
#779=FACE_OUTER_BOUND('',#1471,.T.);
#780=FACE_OUTER_BOUND('',#1472,.T.);
#781=FACE_OUTER_BOUND('',#1473,.T.);
#782=FACE_OUTER_BOUND('',#1474,.T.);
#783=FACE_OUTER_BOUND('',#1475,.T.);
#784=FACE_OUTER_BOUND('',#1476,.T.);
#785=FACE_OUTER_BOUND('',#1477,.T.);
#786=FACE_OUTER_BOUND('',#1478,.T.);
#787=FACE_OUTER_BOUND('',#1479,.T.);
#788=FACE_OUTER_BOUND('',#1480,.T.);
#789=FACE_OUTER_BOUND('',#1481,.T.);
#790=FACE_OUTER_BOUND('',#1482,.T.);
#791=FACE_OUTER_BOUND('',#1483,.T.);
#792=FACE_OUTER_BOUND('',#1484,.T.);
#793=FACE_OUTER_BOUND('',#1485,.T.);
#794=FACE_OUTER_BOUND('',#1486,.T.);
#795=FACE_OUTER_BOUND('',#1487,.T.);
#796=FACE_OUTER_BOUND('',#1488,.T.);
#797=FACE_OUTER_BOUND('',#1489,.T.);
#798=FACE_OUTER_BOUND('',#1490,.T.);
#799=FACE_OUTER_BOUND('',#1491,.T.);
#800=FACE_OUTER_BOUND('',#1492,.T.);
#801=FACE_OUTER_BOUND('',#1493,.T.);
#802=FACE_OUTER_BOUND('',#1494,.T.);
#803=FACE_OUTER_BOUND('',#1495,.T.);
#804=FACE_OUTER_BOUND('',#1496,.T.);
#805=FACE_OUTER_BOUND('',#1497,.T.);
#806=FACE_OUTER_BOUND('',#1498,.T.);
#807=FACE_OUTER_BOUND('',#1499,.T.);
#808=FACE_OUTER_BOUND('',#1500,.T.);
#809=FACE_OUTER_BOUND('',#1501,.T.);
#810=FACE_OUTER_BOUND('',#1502,.T.);
#811=FACE_OUTER_BOUND('',#1503,.T.);
#812=FACE_OUTER_BOUND('',#1504,.T.);
#813=FACE_OUTER_BOUND('',#1505,.T.);
#814=FACE_OUTER_BOUND('',#1506,.T.);
#815=FACE_OUTER_BOUND('',#1507,.T.);
#816=FACE_OUTER_BOUND('',#1510,.T.);
#817=FACE_OUTER_BOUND('',#1511,.T.);
#818=FACE_OUTER_BOUND('',#1512,.T.);
#819=FACE_OUTER_BOUND('',#1513,.T.);
#820=FACE_OUTER_BOUND('',#1514,.T.);
#821=FACE_OUTER_BOUND('',#1515,.T.);
#822=FACE_OUTER_BOUND('',#1516,.T.);
#823=FACE_OUTER_BOUND('',#1517,.T.);
#824=FACE_OUTER_BOUND('',#1518,.T.);
#825=FACE_OUTER_BOUND('',#1519,.T.);
#826=FACE_OUTER_BOUND('',#1520,.T.);
#827=FACE_OUTER_BOUND('',#1521,.T.);
#828=FACE_OUTER_BOUND('',#1522,.T.);
#829=FACE_OUTER_BOUND('',#1523,.T.);
#830=FACE_OUTER_BOUND('',#1524,.T.);
#831=FACE_OUTER_BOUND('',#1525,.T.);
#832=FACE_OUTER_BOUND('',#1526,.T.);
#833=FACE_OUTER_BOUND('',#1527,.T.);
#834=FACE_OUTER_BOUND('',#1528,.T.);
#835=FACE_OUTER_BOUND('',#1529,.T.);
#836=FACE_OUTER_BOUND('',#1530,.T.);
#837=FACE_OUTER_BOUND('',#1531,.T.);
#838=FACE_OUTER_BOUND('',#1539,.T.);
#839=FACE_OUTER_BOUND('',#1547,.T.);
#840=FACE_OUTER_BOUND('',#1548,.T.);
#841=FACE_OUTER_BOUND('',#1549,.T.);
#842=FACE_OUTER_BOUND('',#1550,.T.);
#843=FACE_OUTER_BOUND('',#1551,.T.);
#844=FACE_OUTER_BOUND('',#1552,.T.);
#845=FACE_OUTER_BOUND('',#1553,.T.);
#846=FACE_OUTER_BOUND('',#1554,.T.);
#847=FACE_OUTER_BOUND('',#1555,.T.);
#848=FACE_OUTER_BOUND('',#1556,.T.);
#849=FACE_OUTER_BOUND('',#1557,.T.);
#850=FACE_OUTER_BOUND('',#1558,.T.);
#851=FACE_OUTER_BOUND('',#1559,.T.);
#852=FACE_OUTER_BOUND('',#1560,.T.);
#853=FACE_OUTER_BOUND('',#1561,.T.);
#854=FACE_OUTER_BOUND('',#1562,.T.);
#855=FACE_OUTER_BOUND('',#1563,.T.);
#856=FACE_OUTER_BOUND('',#1564,.T.);
#857=FACE_OUTER_BOUND('',#1565,.T.);
#858=FACE_OUTER_BOUND('',#1566,.T.);
#859=FACE_OUTER_BOUND('',#1567,.T.);
#860=FACE_OUTER_BOUND('',#1568,.T.);
#861=FACE_OUTER_BOUND('',#1569,.T.);
#862=FACE_OUTER_BOUND('',#1570,.T.);
#863=FACE_OUTER_BOUND('',#1571,.T.);
#864=FACE_OUTER_BOUND('',#1572,.T.);
#865=FACE_OUTER_BOUND('',#1573,.T.);
#866=FACE_OUTER_BOUND('',#1574,.T.);
#867=FACE_OUTER_BOUND('',#1575,.T.);
#868=FACE_OUTER_BOUND('',#1576,.T.);
#869=FACE_OUTER_BOUND('',#1577,.T.);
#870=FACE_OUTER_BOUND('',#1578,.T.);
#871=FACE_OUTER_BOUND('',#1579,.T.);
#872=FACE_OUTER_BOUND('',#1580,.T.);
#873=FACE_OUTER_BOUND('',#1581,.T.);
#874=FACE_OUTER_BOUND('',#1582,.T.);
#875=FACE_OUTER_BOUND('',#1583,.T.);
#876=FACE_OUTER_BOUND('',#1584,.T.);
#877=FACE_OUTER_BOUND('',#1585,.T.);
#878=FACE_OUTER_BOUND('',#1586,.T.);
#879=FACE_OUTER_BOUND('',#1587,.T.);
#880=FACE_OUTER_BOUND('',#1588,.T.);
#881=FACE_OUTER_BOUND('',#1589,.T.);
#882=FACE_OUTER_BOUND('',#1590,.T.);
#883=FACE_OUTER_BOUND('',#1591,.T.);
#884=FACE_OUTER_BOUND('',#1592,.T.);
#885=FACE_OUTER_BOUND('',#1593,.T.);
#886=FACE_OUTER_BOUND('',#1594,.T.);
#887=FACE_OUTER_BOUND('',#1595,.T.);
#888=FACE_OUTER_BOUND('',#1596,.T.);
#889=FACE_OUTER_BOUND('',#1597,.T.);
#890=FACE_OUTER_BOUND('',#1598,.T.);
#891=FACE_OUTER_BOUND('',#1599,.T.);
#892=FACE_OUTER_BOUND('',#1600,.T.);
#893=FACE_OUTER_BOUND('',#1601,.T.);
#894=FACE_OUTER_BOUND('',#1602,.T.);
#895=FACE_OUTER_BOUND('',#1603,.T.);
#896=FACE_OUTER_BOUND('',#1604,.T.);
#897=FACE_OUTER_BOUND('',#1605,.T.);
#898=FACE_OUTER_BOUND('',#1606,.T.);
#899=FACE_OUTER_BOUND('',#1607,.T.);
#900=FACE_OUTER_BOUND('',#1608,.T.);
#901=FACE_OUTER_BOUND('',#1609,.T.);
#902=FACE_OUTER_BOUND('',#1610,.T.);
#903=FACE_OUTER_BOUND('',#1611,.T.);
#904=FACE_OUTER_BOUND('',#1612,.T.);
#905=FACE_OUTER_BOUND('',#1613,.T.);
#906=FACE_OUTER_BOUND('',#1614,.T.);
#907=FACE_OUTER_BOUND('',#1615,.T.);
#908=FACE_OUTER_BOUND('',#1616,.T.);
#909=FACE_OUTER_BOUND('',#1617,.T.);
#910=FACE_OUTER_BOUND('',#1618,.T.);
#911=FACE_OUTER_BOUND('',#1619,.T.);
#912=FACE_OUTER_BOUND('',#1620,.T.);
#913=FACE_OUTER_BOUND('',#1621,.T.);
#914=FACE_OUTER_BOUND('',#1622,.T.);
#915=FACE_OUTER_BOUND('',#1623,.T.);
#916=FACE_OUTER_BOUND('',#1624,.T.);
#917=FACE_OUTER_BOUND('',#1625,.T.);
#918=FACE_OUTER_BOUND('',#1626,.T.);
#919=FACE_OUTER_BOUND('',#1627,.T.);
#920=FACE_OUTER_BOUND('',#1628,.T.);
#921=FACE_OUTER_BOUND('',#1629,.T.);
#922=FACE_OUTER_BOUND('',#1630,.T.);
#923=FACE_OUTER_BOUND('',#1631,.T.);
#924=FACE_OUTER_BOUND('',#1632,.T.);
#925=FACE_OUTER_BOUND('',#1633,.T.);
#926=FACE_OUTER_BOUND('',#1634,.T.);
#927=FACE_OUTER_BOUND('',#1635,.T.);
#928=FACE_OUTER_BOUND('',#1636,.T.);
#929=FACE_OUTER_BOUND('',#1637,.T.);
#930=FACE_OUTER_BOUND('',#1638,.T.);
#931=FACE_OUTER_BOUND('',#1639,.T.);
#932=FACE_OUTER_BOUND('',#1640,.T.);
#933=FACE_OUTER_BOUND('',#1641,.T.);
#934=FACE_OUTER_BOUND('',#1642,.T.);
#935=FACE_OUTER_BOUND('',#1643,.T.);
#936=FACE_OUTER_BOUND('',#1644,.T.);
#937=FACE_OUTER_BOUND('',#1645,.T.);
#938=FACE_OUTER_BOUND('',#1646,.T.);
#939=FACE_OUTER_BOUND('',#1647,.T.);
#940=FACE_OUTER_BOUND('',#1648,.T.);
#941=FACE_OUTER_BOUND('',#1649,.T.);
#942=FACE_OUTER_BOUND('',#1650,.T.);
#943=FACE_OUTER_BOUND('',#1651,.T.);
#944=FACE_OUTER_BOUND('',#1652,.T.);
#945=FACE_OUTER_BOUND('',#1653,.T.);
#946=FACE_OUTER_BOUND('',#1654,.T.);
#947=FACE_OUTER_BOUND('',#1655,.T.);
#948=FACE_OUTER_BOUND('',#1656,.T.);
#949=FACE_OUTER_BOUND('',#1657,.T.);
#950=FACE_OUTER_BOUND('',#1658,.T.);
#951=FACE_OUTER_BOUND('',#1659,.T.);
#952=FACE_OUTER_BOUND('',#1660,.T.);
#953=FACE_OUTER_BOUND('',#1661,.T.);
#954=FACE_OUTER_BOUND('',#1662,.T.);
#955=FACE_OUTER_BOUND('',#1663,.T.);
#956=FACE_OUTER_BOUND('',#1664,.T.);
#957=FACE_OUTER_BOUND('',#1665,.T.);
#958=FACE_OUTER_BOUND('',#1675,.T.);
#959=FACE_OUTER_BOUND('',#1676,.T.);
#960=FACE_OUTER_BOUND('',#1677,.T.);
#961=FACE_OUTER_BOUND('',#1678,.T.);
#962=FACE_OUTER_BOUND('',#1679,.T.);
#963=FACE_OUTER_BOUND('',#1680,.T.);
#964=FACE_OUTER_BOUND('',#1681,.T.);
#965=FACE_OUTER_BOUND('',#1682,.T.);
#966=FACE_OUTER_BOUND('',#1683,.T.);
#967=FACE_OUTER_BOUND('',#1684,.T.);
#968=FACE_OUTER_BOUND('',#1685,.T.);
#969=FACE_OUTER_BOUND('',#1686,.T.);
#970=FACE_OUTER_BOUND('',#1687,.T.);
#971=FACE_OUTER_BOUND('',#1689,.T.);
#972=FACE_OUTER_BOUND('',#1691,.T.);
#973=FACE_OUTER_BOUND('',#1693,.T.);
#974=FACE_OUTER_BOUND('',#1695,.T.);
#975=FACE_OUTER_BOUND('',#1696,.T.);
#976=FACE_OUTER_BOUND('',#1697,.T.);
#977=FACE_OUTER_BOUND('',#1698,.T.);
#978=FACE_OUTER_BOUND('',#1699,.T.);
#979=FACE_OUTER_BOUND('',#1700,.T.);
#980=FACE_OUTER_BOUND('',#1701,.T.);
#981=FACE_OUTER_BOUND('',#1702,.T.);
#982=FACE_OUTER_BOUND('',#1703,.T.);
#983=FACE_OUTER_BOUND('',#1704,.T.);
#984=FACE_OUTER_BOUND('',#1705,.T.);
#985=FACE_OUTER_BOUND('',#1706,.T.);
#986=FACE_OUTER_BOUND('',#1707,.T.);
#987=FACE_OUTER_BOUND('',#1708,.T.);
#988=FACE_OUTER_BOUND('',#1709,.T.);
#989=FACE_OUTER_BOUND('',#1710,.T.);
#990=FACE_OUTER_BOUND('',#1711,.T.);
#991=FACE_OUTER_BOUND('',#1712,.T.);
#992=FACE_OUTER_BOUND('',#1713,.T.);
#993=FACE_OUTER_BOUND('',#1714,.T.);
#994=FACE_OUTER_BOUND('',#1715,.T.);
#995=FACE_OUTER_BOUND('',#1716,.T.);
#996=FACE_OUTER_BOUND('',#1717,.T.);
#997=FACE_OUTER_BOUND('',#1718,.T.);
#998=FACE_OUTER_BOUND('',#1719,.T.);
#999=FACE_OUTER_BOUND('',#1720,.T.);
#1000=FACE_OUTER_BOUND('',#1721,.T.);
#1001=FACE_OUTER_BOUND('',#1722,.T.);
#1002=FACE_OUTER_BOUND('',#1723,.T.);
#1003=FACE_OUTER_BOUND('',#1724,.T.);
#1004=FACE_OUTER_BOUND('',#1725,.T.);
#1005=FACE_OUTER_BOUND('',#1726,.T.);
#1006=FACE_OUTER_BOUND('',#1727,.T.);
#1007=FACE_OUTER_BOUND('',#1728,.T.);
#1008=FACE_OUTER_BOUND('',#1729,.T.);
#1009=FACE_OUTER_BOUND('',#1730,.T.);
#1010=FACE_OUTER_BOUND('',#1731,.T.);
#1011=FACE_OUTER_BOUND('',#1732,.T.);
#1012=FACE_OUTER_BOUND('',#1733,.T.);
#1013=FACE_OUTER_BOUND('',#1734,.T.);
#1014=FACE_OUTER_BOUND('',#1735,.T.);
#1015=FACE_OUTER_BOUND('',#1736,.T.);
#1016=FACE_OUTER_BOUND('',#1737,.T.);
#1017=FACE_OUTER_BOUND('',#1738,.T.);
#1018=FACE_OUTER_BOUND('',#1739,.T.);
#1019=FACE_OUTER_BOUND('',#1740,.T.);
#1020=FACE_OUTER_BOUND('',#1741,.T.);
#1021=FACE_OUTER_BOUND('',#1742,.T.);
#1022=FACE_OUTER_BOUND('',#1743,.T.);
#1023=FACE_OUTER_BOUND('',#1744,.T.);
#1024=FACE_OUTER_BOUND('',#1745,.T.);
#1025=FACE_OUTER_BOUND('',#1746,.T.);
#1026=FACE_OUTER_BOUND('',#1747,.T.);
#1027=FACE_OUTER_BOUND('',#1748,.T.);
#1028=FACE_OUTER_BOUND('',#1749,.T.);
#1029=FACE_OUTER_BOUND('',#1750,.T.);
#1030=FACE_OUTER_BOUND('',#1751,.T.);
#1031=FACE_OUTER_BOUND('',#1752,.T.);
#1032=FACE_OUTER_BOUND('',#1753,.T.);
#1033=FACE_OUTER_BOUND('',#1754,.T.);
#1034=FACE_OUTER_BOUND('',#1755,.T.);
#1035=FACE_OUTER_BOUND('',#1756,.T.);
#1036=FACE_OUTER_BOUND('',#1757,.T.);
#1037=FACE_OUTER_BOUND('',#1758,.T.);
#1038=FACE_OUTER_BOUND('',#1759,.T.);
#1039=FACE_OUTER_BOUND('',#1760,.T.);
#1040=FACE_OUTER_BOUND('',#1761,.T.);
#1041=FACE_OUTER_BOUND('',#1762,.T.);
#1042=FACE_OUTER_BOUND('',#1763,.T.);
#1043=FACE_OUTER_BOUND('',#1764,.T.);
#1044=FACE_OUTER_BOUND('',#1765,.T.);
#1045=FACE_OUTER_BOUND('',#1767,.T.);
#1046=FACE_OUTER_BOUND('',#1768,.T.);
#1047=FACE_OUTER_BOUND('',#1769,.T.);
#1048=FACE_OUTER_BOUND('',#1770,.T.);
#1049=FACE_OUTER_BOUND('',#1771,.T.);
#1050=FACE_OUTER_BOUND('',#1772,.T.);
#1051=FACE_OUTER_BOUND('',#1773,.T.);
#1052=FACE_OUTER_BOUND('',#1774,.T.);
#1053=FACE_OUTER_BOUND('',#1775,.T.);
#1054=FACE_OUTER_BOUND('',#1776,.T.);
#1055=FACE_OUTER_BOUND('',#1777,.T.);
#1056=FACE_OUTER_BOUND('',#1778,.T.);
#1057=FACE_OUTER_BOUND('',#1779,.T.);
#1058=FACE_OUTER_BOUND('',#1780,.T.);
#1059=FACE_OUTER_BOUND('',#1781,.T.);
#1060=FACE_OUTER_BOUND('',#1782,.T.);
#1061=FACE_OUTER_BOUND('',#1783,.T.);
#1062=FACE_OUTER_BOUND('',#1784,.T.);
#1063=FACE_OUTER_BOUND('',#1785,.T.);
#1064=FACE_OUTER_BOUND('',#1786,.T.);
#1065=FACE_OUTER_BOUND('',#1794,.T.);
#1066=FACE_OUTER_BOUND('',#1802,.T.);
#1067=FACE_OUTER_BOUND('',#1803,.T.);
#1068=FACE_OUTER_BOUND('',#1804,.T.);
#1069=FACE_OUTER_BOUND('',#1805,.T.);
#1070=FACE_OUTER_BOUND('',#1806,.T.);
#1071=FACE_OUTER_BOUND('',#1807,.T.);
#1072=FACE_OUTER_BOUND('',#1808,.T.);
#1073=FACE_OUTER_BOUND('',#1809,.T.);
#1074=FACE_OUTER_BOUND('',#1810,.T.);
#1075=FACE_OUTER_BOUND('',#1811,.T.);
#1076=FACE_OUTER_BOUND('',#1812,.T.);
#1077=FACE_OUTER_BOUND('',#1813,.T.);
#1078=FACE_OUTER_BOUND('',#1814,.T.);
#1079=FACE_OUTER_BOUND('',#1815,.T.);
#1080=FACE_OUTER_BOUND('',#1816,.T.);
#1081=FACE_OUTER_BOUND('',#1817,.T.);
#1082=FACE_OUTER_BOUND('',#1818,.T.);
#1083=FACE_OUTER_BOUND('',#1819,.T.);
#1084=FACE_OUTER_BOUND('',#1820,.T.);
#1085=FACE_OUTER_BOUND('',#1821,.T.);
#1086=FACE_OUTER_BOUND('',#1822,.T.);
#1087=FACE_OUTER_BOUND('',#1823,.T.);
#1088=FACE_OUTER_BOUND('',#1824,.T.);
#1089=FACE_OUTER_BOUND('',#1825,.T.);
#1090=FACE_OUTER_BOUND('',#1826,.T.);
#1091=FACE_OUTER_BOUND('',#1827,.T.);
#1092=FACE_OUTER_BOUND('',#1828,.T.);
#1093=FACE_OUTER_BOUND('',#1829,.T.);
#1094=FACE_OUTER_BOUND('',#1830,.T.);
#1095=FACE_OUTER_BOUND('',#1831,.T.);
#1096=FACE_OUTER_BOUND('',#1832,.T.);
#1097=FACE_OUTER_BOUND('',#1833,.T.);
#1098=FACE_OUTER_BOUND('',#1834,.T.);
#1099=FACE_OUTER_BOUND('',#1835,.T.);
#1100=FACE_OUTER_BOUND('',#1836,.T.);
#1101=FACE_OUTER_BOUND('',#1837,.T.);
#1102=FACE_OUTER_BOUND('',#1838,.T.);
#1103=FACE_OUTER_BOUND('',#1839,.T.);
#1104=FACE_OUTER_BOUND('',#1840,.T.);
#1105=FACE_OUTER_BOUND('',#1841,.T.);
#1106=FACE_OUTER_BOUND('',#1842,.T.);
#1107=FACE_OUTER_BOUND('',#1843,.T.);
#1108=FACE_OUTER_BOUND('',#1844,.T.);
#1109=FACE_OUTER_BOUND('',#1845,.T.);
#1110=FACE_OUTER_BOUND('',#1846,.T.);
#1111=FACE_OUTER_BOUND('',#1847,.T.);
#1112=FACE_OUTER_BOUND('',#1848,.T.);
#1113=FACE_OUTER_BOUND('',#1849,.T.);
#1114=FACE_OUTER_BOUND('',#1850,.T.);
#1115=FACE_OUTER_BOUND('',#1851,.T.);
#1116=FACE_OUTER_BOUND('',#1852,.T.);
#1117=FACE_OUTER_BOUND('',#1853,.T.);
#1118=FACE_OUTER_BOUND('',#1854,.T.);
#1119=FACE_OUTER_BOUND('',#1855,.T.);
#1120=FACE_OUTER_BOUND('',#1856,.T.);
#1121=FACE_OUTER_BOUND('',#1857,.T.);
#1122=FACE_OUTER_BOUND('',#1858,.T.);
#1123=FACE_OUTER_BOUND('',#1859,.T.);
#1124=FACE_OUTER_BOUND('',#1860,.T.);
#1125=FACE_OUTER_BOUND('',#1861,.T.);
#1126=FACE_OUTER_BOUND('',#1862,.T.);
#1127=FACE_OUTER_BOUND('',#1863,.T.);
#1128=FACE_OUTER_BOUND('',#1864,.T.);
#1129=FACE_OUTER_BOUND('',#1865,.T.);
#1130=FACE_OUTER_BOUND('',#1866,.T.);
#1131=FACE_OUTER_BOUND('',#1867,.T.);
#1132=FACE_OUTER_BOUND('',#1868,.T.);
#1133=FACE_OUTER_BOUND('',#1869,.T.);
#1134=FACE_OUTER_BOUND('',#1870,.T.);
#1135=FACE_OUTER_BOUND('',#1871,.T.);
#1136=FACE_OUTER_BOUND('',#1872,.T.);
#1137=FACE_OUTER_BOUND('',#1873,.T.);
#1138=FACE_OUTER_BOUND('',#1874,.T.);
#1139=FACE_OUTER_BOUND('',#1875,.T.);
#1140=FACE_OUTER_BOUND('',#1876,.T.);
#1141=FACE_OUTER_BOUND('',#1877,.T.);
#1142=FACE_OUTER_BOUND('',#1878,.T.);
#1143=FACE_OUTER_BOUND('',#1879,.T.);
#1144=FACE_OUTER_BOUND('',#1880,.T.);
#1145=FACE_OUTER_BOUND('',#1881,.T.);
#1146=FACE_OUTER_BOUND('',#1882,.T.);
#1147=FACE_OUTER_BOUND('',#1883,.T.);
#1148=FACE_OUTER_BOUND('',#1884,.T.);
#1149=FACE_OUTER_BOUND('',#1885,.T.);
#1150=FACE_OUTER_BOUND('',#1886,.T.);
#1151=FACE_OUTER_BOUND('',#1887,.T.);
#1152=FACE_OUTER_BOUND('',#1888,.T.);
#1153=FACE_OUTER_BOUND('',#1889,.T.);
#1154=FACE_OUTER_BOUND('',#1890,.T.);
#1155=FACE_OUTER_BOUND('',#1891,.T.);
#1156=FACE_OUTER_BOUND('',#1892,.T.);
#1157=FACE_OUTER_BOUND('',#1893,.T.);
#1158=FACE_OUTER_BOUND('',#1894,.T.);
#1159=FACE_OUTER_BOUND('',#1895,.T.);
#1160=FACE_OUTER_BOUND('',#1896,.T.);
#1161=FACE_OUTER_BOUND('',#1897,.T.);
#1162=FACE_OUTER_BOUND('',#1898,.T.);
#1163=FACE_OUTER_BOUND('',#1899,.T.);
#1164=FACE_OUTER_BOUND('',#1900,.T.);
#1165=FACE_OUTER_BOUND('',#1901,.T.);
#1166=FACE_OUTER_BOUND('',#1902,.T.);
#1167=FACE_OUTER_BOUND('',#1903,.T.);
#1168=FACE_OUTER_BOUND('',#1904,.T.);
#1169=FACE_OUTER_BOUND('',#1905,.T.);
#1170=FACE_OUTER_BOUND('',#1906,.T.);
#1171=FACE_OUTER_BOUND('',#1907,.T.);
#1172=FACE_OUTER_BOUND('',#1908,.T.);
#1173=FACE_OUTER_BOUND('',#1909,.T.);
#1174=FACE_OUTER_BOUND('',#1910,.T.);
#1175=FACE_OUTER_BOUND('',#1911,.T.);
#1176=FACE_OUTER_BOUND('',#1912,.T.);
#1177=FACE_OUTER_BOUND('',#1913,.T.);
#1178=FACE_OUTER_BOUND('',#1914,.T.);
#1179=FACE_OUTER_BOUND('',#1915,.T.);
#1180=FACE_OUTER_BOUND('',#1916,.T.);
#1181=FACE_OUTER_BOUND('',#1917,.T.);
#1182=FACE_OUTER_BOUND('',#1918,.T.);
#1183=FACE_OUTER_BOUND('',#1919,.T.);
#1184=FACE_OUTER_BOUND('',#1920,.T.);
#1185=FACE_OUTER_BOUND('',#1921,.T.);
#1186=FACE_OUTER_BOUND('',#1922,.T.);
#1187=FACE_OUTER_BOUND('',#1923,.T.);
#1188=FACE_OUTER_BOUND('',#1924,.T.);
#1189=FACE_OUTER_BOUND('',#1925,.T.);
#1190=FACE_OUTER_BOUND('',#1926,.T.);
#1191=FACE_OUTER_BOUND('',#1927,.T.);
#1192=FACE_OUTER_BOUND('',#1928,.T.);
#1193=FACE_OUTER_BOUND('',#1929,.T.);
#1194=FACE_OUTER_BOUND('',#1930,.T.);
#1195=FACE_OUTER_BOUND('',#1931,.T.);
#1196=FACE_OUTER_BOUND('',#1932,.T.);
#1197=FACE_OUTER_BOUND('',#1933,.T.);
#1198=FACE_OUTER_BOUND('',#1934,.T.);
#1199=FACE_OUTER_BOUND('',#1935,.T.);
#1200=FACE_OUTER_BOUND('',#1936,.T.);
#1201=FACE_OUTER_BOUND('',#1937,.T.);
#1202=FACE_OUTER_BOUND('',#1938,.T.);
#1203=FACE_OUTER_BOUND('',#1939,.T.);
#1204=FACE_OUTER_BOUND('',#1940,.T.);
#1205=FACE_OUTER_BOUND('',#1941,.T.);
#1206=FACE_OUTER_BOUND('',#1942,.T.);
#1207=FACE_OUTER_BOUND('',#1943,.T.);
#1208=FACE_OUTER_BOUND('',#1944,.T.);
#1209=FACE_OUTER_BOUND('',#1945,.T.);
#1210=FACE_OUTER_BOUND('',#1946,.T.);
#1211=FACE_OUTER_BOUND('',#1947,.T.);
#1212=FACE_OUTER_BOUND('',#1948,.T.);
#1213=FACE_OUTER_BOUND('',#1949,.T.);
#1214=FACE_OUTER_BOUND('',#1950,.T.);
#1215=FACE_OUTER_BOUND('',#1951,.T.);
#1216=FACE_OUTER_BOUND('',#1952,.T.);
#1217=FACE_OUTER_BOUND('',#1953,.T.);
#1218=FACE_OUTER_BOUND('',#1954,.T.);
#1219=FACE_OUTER_BOUND('',#1955,.T.);
#1220=FACE_OUTER_BOUND('',#1956,.T.);
#1221=FACE_OUTER_BOUND('',#1957,.T.);
#1222=FACE_OUTER_BOUND('',#1958,.T.);
#1223=FACE_OUTER_BOUND('',#1959,.T.);
#1224=FACE_OUTER_BOUND('',#1960,.T.);
#1225=FACE_OUTER_BOUND('',#1961,.T.);
#1226=FACE_OUTER_BOUND('',#1962,.T.);
#1227=FACE_OUTER_BOUND('',#1963,.T.);
#1228=FACE_OUTER_BOUND('',#1964,.T.);
#1229=FACE_OUTER_BOUND('',#1965,.T.);
#1230=FACE_OUTER_BOUND('',#1966,.T.);
#1231=FACE_OUTER_BOUND('',#1967,.T.);
#1232=FACE_OUTER_BOUND('',#1968,.T.);
#1233=FACE_OUTER_BOUND('',#1969,.T.);
#1234=FACE_OUTER_BOUND('',#1970,.T.);
#1235=FACE_OUTER_BOUND('',#1971,.T.);
#1236=FACE_OUTER_BOUND('',#1972,.T.);
#1237=FACE_OUTER_BOUND('',#1973,.T.);
#1238=FACE_OUTER_BOUND('',#1974,.T.);
#1239=FACE_OUTER_BOUND('',#1975,.T.);
#1240=FACE_OUTER_BOUND('',#1976,.T.);
#1241=FACE_OUTER_BOUND('',#1977,.T.);
#1242=FACE_OUTER_BOUND('',#1978,.T.);
#1243=FACE_OUTER_BOUND('',#1979,.T.);
#1244=FACE_OUTER_BOUND('',#1980,.T.);
#1245=FACE_OUTER_BOUND('',#1981,.T.);
#1246=FACE_OUTER_BOUND('',#1982,.T.);
#1247=FACE_OUTER_BOUND('',#1983,.T.);
#1248=FACE_OUTER_BOUND('',#1984,.T.);
#1249=FACE_OUTER_BOUND('',#1985,.T.);
#1250=FACE_OUTER_BOUND('',#1986,.T.);
#1251=FACE_OUTER_BOUND('',#1987,.T.);
#1252=FACE_OUTER_BOUND('',#1988,.T.);
#1253=FACE_OUTER_BOUND('',#1989,.T.);
#1254=FACE_OUTER_BOUND('',#1990,.T.);
#1255=FACE_OUTER_BOUND('',#1991,.T.);
#1256=FACE_OUTER_BOUND('',#1992,.T.);
#1257=FACE_OUTER_BOUND('',#1993,.T.);
#1258=FACE_OUTER_BOUND('',#1994,.T.);
#1259=FACE_OUTER_BOUND('',#1995,.T.);
#1260=FACE_OUTER_BOUND('',#1996,.T.);
#1261=FACE_OUTER_BOUND('',#1997,.T.);
#1262=FACE_OUTER_BOUND('',#1998,.T.);
#1263=FACE_OUTER_BOUND('',#1999,.T.);
#1264=FACE_OUTER_BOUND('',#2000,.T.);
#1265=FACE_OUTER_BOUND('',#2001,.T.);
#1266=FACE_OUTER_BOUND('',#2002,.T.);
#1267=FACE_OUTER_BOUND('',#2003,.T.);
#1268=FACE_OUTER_BOUND('',#2004,.T.);
#1269=FACE_OUTER_BOUND('',#2005,.T.);
#1270=FACE_OUTER_BOUND('',#2006,.T.);
#1271=FACE_OUTER_BOUND('',#2007,.T.);
#1272=FACE_OUTER_BOUND('',#2008,.T.);
#1273=FACE_OUTER_BOUND('',#2009,.T.);
#1274=FACE_OUTER_BOUND('',#2010,.T.);
#1275=FACE_OUTER_BOUND('',#2011,.T.);
#1276=FACE_OUTER_BOUND('',#2012,.T.);
#1277=FACE_OUTER_BOUND('',#2013,.T.);
#1278=FACE_OUTER_BOUND('',#2014,.T.);
#1279=FACE_OUTER_BOUND('',#2015,.T.);
#1280=FACE_OUTER_BOUND('',#2016,.T.);
#1281=FACE_OUTER_BOUND('',#2017,.T.);
#1282=FACE_OUTER_BOUND('',#2018,.T.);
#1283=FACE_OUTER_BOUND('',#2019,.T.);
#1284=FACE_OUTER_BOUND('',#2020,.T.);
#1285=FACE_OUTER_BOUND('',#2021,.T.);
#1286=FACE_OUTER_BOUND('',#2022,.T.);
#1287=FACE_OUTER_BOUND('',#2023,.T.);
#1288=FACE_OUTER_BOUND('',#2024,.T.);
#1289=FACE_OUTER_BOUND('',#2025,.T.);
#1290=FACE_OUTER_BOUND('',#2026,.T.);
#1291=FACE_OUTER_BOUND('',#2027,.T.);
#1292=FACE_OUTER_BOUND('',#2028,.T.);
#1293=FACE_OUTER_BOUND('',#2029,.T.);
#1294=FACE_OUTER_BOUND('',#2030,.T.);
#1295=FACE_OUTER_BOUND('',#2031,.T.);
#1296=FACE_OUTER_BOUND('',#2032,.T.);
#1297=FACE_OUTER_BOUND('',#2033,.T.);
#1298=FACE_OUTER_BOUND('',#2034,.T.);
#1299=FACE_OUTER_BOUND('',#2035,.T.);
#1300=FACE_OUTER_BOUND('',#2036,.T.);
#1301=FACE_OUTER_BOUND('',#2037,.T.);
#1302=FACE_OUTER_BOUND('',#2038,.T.);
#1303=FACE_OUTER_BOUND('',#2039,.T.);
#1304=FACE_OUTER_BOUND('',#2040,.T.);
#1305=FACE_OUTER_BOUND('',#2041,.T.);
#1306=FACE_OUTER_BOUND('',#2042,.T.);
#1307=FACE_OUTER_BOUND('',#2043,.T.);
#1308=FACE_OUTER_BOUND('',#2044,.T.);
#1309=FACE_OUTER_BOUND('',#2045,.T.);
#1310=FACE_OUTER_BOUND('',#2046,.T.);
#1311=FACE_OUTER_BOUND('',#2047,.T.);
#1312=FACE_OUTER_BOUND('',#2048,.T.);
#1313=FACE_OUTER_BOUND('',#2049,.T.);
#1314=FACE_OUTER_BOUND('',#2050,.T.);
#1315=FACE_OUTER_BOUND('',#2051,.T.);
#1316=FACE_OUTER_BOUND('',#2052,.T.);
#1317=FACE_OUTER_BOUND('',#2053,.T.);
#1318=FACE_OUTER_BOUND('',#2054,.T.);
#1319=FACE_OUTER_BOUND('',#2055,.T.);
#1320=FACE_OUTER_BOUND('',#2056,.T.);
#1321=FACE_OUTER_BOUND('',#2057,.T.);
#1322=FACE_OUTER_BOUND('',#2058,.T.);
#1323=FACE_OUTER_BOUND('',#2059,.T.);
#1324=FACE_OUTER_BOUND('',#2060,.T.);
#1325=FACE_OUTER_BOUND('',#2065,.T.);
#1326=FACE_OUTER_BOUND('',#2070,.T.);
#1327=FACE_OUTER_BOUND('',#2071,.T.);
#1328=FACE_OUTER_BOUND('',#2072,.T.);
#1329=FACE_OUTER_BOUND('',#2073,.T.);
#1330=FACE_OUTER_BOUND('',#2074,.T.);
#1331=FACE_OUTER_BOUND('',#2075,.T.);
#1332=FACE_OUTER_BOUND('',#2076,.T.);
#1333=FACE_OUTER_BOUND('',#2077,.T.);
#1334=FACE_OUTER_BOUND('',#2078,.T.);
#1335=FACE_OUTER_BOUND('',#2079,.T.);
#1336=FACE_OUTER_BOUND('',#2080,.T.);
#1337=FACE_OUTER_BOUND('',#2081,.T.);
#1338=FACE_OUTER_BOUND('',#2082,.T.);
#1339=FACE_OUTER_BOUND('',#2083,.T.);
#1340=FACE_OUTER_BOUND('',#2084,.T.);
#1341=FACE_OUTER_BOUND('',#2085,.T.);
#1342=FACE_OUTER_BOUND('',#2086,.T.);
#1343=FACE_OUTER_BOUND('',#2087,.T.);
#1344=FACE_OUTER_BOUND('',#2088,.T.);
#1345=FACE_OUTER_BOUND('',#2089,.T.);
#1346=FACE_OUTER_BOUND('',#2090,.T.);
#1347=FACE_OUTER_BOUND('',#2091,.T.);
#1348=FACE_OUTER_BOUND('',#2092,.T.);
#1349=FACE_OUTER_BOUND('',#2093,.T.);
#1350=FACE_OUTER_BOUND('',#2096,.T.);
#1351=FACE_OUTER_BOUND('',#2097,.T.);
#1352=FACE_OUTER_BOUND('',#2098,.T.);
#1353=FACE_OUTER_BOUND('',#2099,.T.);
#1354=FACE_OUTER_BOUND('',#2100,.T.);
#1355=FACE_OUTER_BOUND('',#2101,.T.);
#1356=FACE_OUTER_BOUND('',#2104,.T.);
#1357=FACE_OUTER_BOUND('',#2105,.T.);
#1358=FACE_OUTER_BOUND('',#2106,.T.);
#1359=FACE_OUTER_BOUND('',#2107,.T.);
#1360=FACE_OUTER_BOUND('',#2108,.T.);
#1361=FACE_OUTER_BOUND('',#2111,.T.);
#1362=FACE_OUTER_BOUND('',#2112,.T.);
#1363=FACE_OUTER_BOUND('',#2113,.T.);
#1364=FACE_OUTER_BOUND('',#2116,.T.);
#1365=FACE_OUTER_BOUND('',#2117,.T.);
#1366=FACE_OUTER_BOUND('',#2118,.T.);
#1367=FACE_OUTER_BOUND('',#2119,.T.);
#1368=FACE_OUTER_BOUND('',#2120,.T.);
#1369=FACE_OUTER_BOUND('',#2121,.T.);
#1370=FACE_OUTER_BOUND('',#2122,.T.);
#1371=FACE_OUTER_BOUND('',#2123,.T.);
#1372=FACE_OUTER_BOUND('',#2124,.T.);
#1373=FACE_OUTER_BOUND('',#2125,.T.);
#1374=FACE_OUTER_BOUND('',#2128,.T.);
#1375=FACE_OUTER_BOUND('',#2129,.T.);
#1376=FACE_OUTER_BOUND('',#2130,.T.);
#1377=FACE_OUTER_BOUND('',#2133,.T.);
#1378=FACE_OUTER_BOUND('',#2134,.T.);
#1379=FACE_OUTER_BOUND('',#2135,.T.);
#1380=FACE_OUTER_BOUND('',#2136,.T.);
#1381=FACE_OUTER_BOUND('',#2137,.T.);
#1382=FACE_OUTER_BOUND('',#2138,.T.);
#1383=FACE_OUTER_BOUND('',#2139,.T.);
#1384=EDGE_LOOP('',(#7528,#7529,#7530));
#1385=EDGE_LOOP('',(#7531,#7532,#7533,#7534,#7535));
#1386=EDGE_LOOP('',(#7536,#7537,#7538,#7539));
#1387=EDGE_LOOP('',(#7540,#7541,#7542,#7543,#7544));
#1388=EDGE_LOOP('',(#7545,#7546,#7547,#7548));
#1389=EDGE_LOOP('',(#7549,#7550,#7551));
#1390=EDGE_LOOP('',(#7552,#7553,#7554));
#1391=EDGE_LOOP('',(#7555,#7556,#7557));
#1392=EDGE_LOOP('',(#7558,#7559,#7560));
#1393=EDGE_LOOP('',(#7561,#7562,#7563,#7564,#7565));
#1394=EDGE_LOOP('',(#7566,#7567,#7568,#7569,#7570));
#1395=EDGE_LOOP('',(#7571,#7572,#7573,#7574));
#1396=EDGE_LOOP('',(#7575,#7576,#7577,#7578));
#1397=EDGE_LOOP('',(#7579,#7580,#7581,#7582));
#1398=EDGE_LOOP('',(#7583,#7584,#7585,#7586));
#1399=EDGE_LOOP('',(#7587,#7588,#7589,#7590));
#1400=EDGE_LOOP('',(#7591,#7592,#7593,#7594));
#1401=EDGE_LOOP('',(#7595,#7596,#7597,#7598));
#1402=EDGE_LOOP('',(#7599,#7600,#7601,#7602));
#1403=EDGE_LOOP('',(#7603,#7604,#7605,#7606));
#1404=EDGE_LOOP('',(#7607,#7608,#7609,#7610));
#1405=EDGE_LOOP('',(#7611,#7612,#7613,#7614));
#1406=EDGE_LOOP('',(#7615,#7616,#7617,#7618));
#1407=EDGE_LOOP('',(#7619,#7620,#7621,#7622,#7623,#7624));
#1408=EDGE_LOOP('',(#7625,#7626,#7627,#7628));
#1409=EDGE_LOOP('',(#7629,#7630,#7631,#7632,#7633));
#1410=EDGE_LOOP('',(#7634,#7635,#7636,#7637,#7638));
#1411=EDGE_LOOP('',(#7639,#7640,#7641,#7642));
#1412=EDGE_LOOP('',(#7643,#7644,#7645,#7646));
#1413=EDGE_LOOP('',(#7647,#7648,#7649,#7650));
#1414=EDGE_LOOP('',(#7651,#7652,#7653,#7654));
#1415=EDGE_LOOP('',(#7655,#7656,#7657,#7658));
#1416=EDGE_LOOP('',(#7659,#7660,#7661,#7662,#7663,#7664,#7665,#7666,#7667,
#7668,#7669));
#1417=EDGE_LOOP('',(#7670,#7671,#7672,#7673,#7674,#7675));
#1418=EDGE_LOOP('',(#7676,#7677,#7678,#7679,#7680,#7681,#7682,#7683,#7684,
#7685,#7686,#7687,#7688,#7689,#7690));
#1419=EDGE_LOOP('',(#7691,#7692,#7693,#7694,#7695,#7696,#7697,#7698,#7699,
#7700,#7701,#7702,#7703,#7704,#7705,#7706,#7707,#7708,#7709,#7710));
#1420=EDGE_LOOP('',(#7711,#7712,#7713,#7714,#7715,#7716,#7717,#7718,#7719,
#7720,#7721,#7722,#7723,#7724,#7725,#7726,#7727,#7728,#7729,#7730));
#1421=EDGE_LOOP('',(#7731,#7732,#7733,#7734,#7735,#7736));
#1422=EDGE_LOOP('',(#7737));
#1423=EDGE_LOOP('',(#7738));
#1424=EDGE_LOOP('',(#7739,#7740,#7741,#7742,#7743,#7744,#7745,#7746,#7747,
#7748,#7749,#7750,#7751,#7752,#7753,#7754,#7755,#7756));
#1425=EDGE_LOOP('',(#7757));
#1426=EDGE_LOOP('',(#7758));
#1427=EDGE_LOOP('',(#7759,#7760,#7761,#7762,#7763,#7764,#7765,#7766,#7767,
#7768,#7769,#7770,#7771,#7772,#7773,#7774,#7775,#7776));
#1428=EDGE_LOOP('',(#7777));
#1429=EDGE_LOOP('',(#7778));
#1430=EDGE_LOOP('',(#7779));
#1431=EDGE_LOOP('',(#7780));
#1432=EDGE_LOOP('',(#7781,#7782,#7783,#7784));
#1433=EDGE_LOOP('',(#7785,#7786,#7787,#7788,#7789));
#1434=EDGE_LOOP('',(#7790,#7791,#7792,#7793,#7794,#7795));
#1435=EDGE_LOOP('',(#7796,#7797,#7798,#7799,#7800));
#1436=EDGE_LOOP('',(#7801,#7802,#7803,#7804,#7805,#7806,#7807,#7808));
#1437=EDGE_LOOP('',(#7809,#7810,#7811,#7812,#7813,#7814,#7815,#7816));
#1438=EDGE_LOOP('',(#7817,#7818,#7819,#7820,#7821,#7822));
#1439=EDGE_LOOP('',(#7823,#7824,#7825,#7826,#7827));
#1440=EDGE_LOOP('',(#7828,#7829,#7830,#7831,#7832));
#1441=EDGE_LOOP('',(#7833,#7834,#7835,#7836));
#1442=EDGE_LOOP('',(#7837,#7838,#7839,#7840,#7841));
#1443=EDGE_LOOP('',(#7842,#7843,#7844,#7845,#7846,#7847,#7848,#7849));
#1444=EDGE_LOOP('',(#7850,#7851,#7852,#7853,#7854));
#1445=EDGE_LOOP('',(#7855,#7856,#7857,#7858));
#1446=EDGE_LOOP('',(#7859,#7860,#7861,#7862));
#1447=EDGE_LOOP('',(#7863,#7864,#7865,#7866));
#1448=EDGE_LOOP('',(#7867,#7868,#7869,#7870));
#1449=EDGE_LOOP('',(#7871,#7872,#7873,#7874));
#1450=EDGE_LOOP('',(#7875,#7876,#7877,#7878));
#1451=EDGE_LOOP('',(#7879,#7880,#7881,#7882));
#1452=EDGE_LOOP('',(#7883,#7884,#7885,#7886));
#1453=EDGE_LOOP('',(#7887,#7888,#7889,#7890));
#1454=EDGE_LOOP('',(#7891,#7892,#7893,#7894));
#1455=EDGE_LOOP('',(#7895,#7896,#7897,#7898));
#1456=EDGE_LOOP('',(#7899,#7900,#7901,#7902));
#1457=EDGE_LOOP('',(#7903,#7904,#7905,#7906));
#1458=EDGE_LOOP('',(#7907,#7908,#7909,#7910));
#1459=EDGE_LOOP('',(#7911,#7912,#7913,#7914));
#1460=EDGE_LOOP('',(#7915,#7916,#7917,#7918));
#1461=EDGE_LOOP('',(#7919,#7920,#7921,#7922));
#1462=EDGE_LOOP('',(#7923,#7924,#7925,#7926));
#1463=EDGE_LOOP('',(#7927,#7928,#7929));
#1464=EDGE_LOOP('',(#7930,#7931,#7932,#7933));
#1465=EDGE_LOOP('',(#7934,#7935,#7936,#7937,#7938));
#1466=EDGE_LOOP('',(#7939,#7940,#7941,#7942,#7943));
#1467=EDGE_LOOP('',(#7944,#7945,#7946,#7947));
#1468=EDGE_LOOP('',(#7948,#7949,#7950));
#1469=EDGE_LOOP('',(#7951,#7952,#7953));
#1470=EDGE_LOOP('',(#7954));
#1471=EDGE_LOOP('',(#7955,#7956,#7957,#7958));
#1472=EDGE_LOOP('',(#7959,#7960,#7961,#7962,#7963));
#1473=EDGE_LOOP('',(#7964,#7965,#7966,#7967,#7968,#7969));
#1474=EDGE_LOOP('',(#7970,#7971,#7972,#7973,#7974));
#1475=EDGE_LOOP('',(#7975,#7976,#7977,#7978,#7979,#7980));
#1476=EDGE_LOOP('',(#7981,#7982,#7983,#7984,#7985));
#1477=EDGE_LOOP('',(#7986,#7987,#7988,#7989,#7990));
#1478=EDGE_LOOP('',(#7991,#7992,#7993,#7994));
#1479=EDGE_LOOP('',(#7995,#7996,#7997,#7998,#7999));
#1480=EDGE_LOOP('',(#8000,#8001,#8002,#8003,#8004,#8005,#8006,#8007));
#1481=EDGE_LOOP('',(#8008,#8009,#8010,#8011,#8012));
#1482=EDGE_LOOP('',(#8013,#8014,#8015,#8016));
#1483=EDGE_LOOP('',(#8017,#8018,#8019,#8020));
#1484=EDGE_LOOP('',(#8021,#8022,#8023,#8024));
#1485=EDGE_LOOP('',(#8025,#8026,#8027,#8028));
#1486=EDGE_LOOP('',(#8029,#8030,#8031,#8032));
#1487=EDGE_LOOP('',(#8033,#8034,#8035,#8036));
#1488=EDGE_LOOP('',(#8037,#8038,#8039,#8040));
#1489=EDGE_LOOP('',(#8041,#8042,#8043,#8044));
#1490=EDGE_LOOP('',(#8045,#8046,#8047,#8048));
#1491=EDGE_LOOP('',(#8049,#8050,#8051,#8052));
#1492=EDGE_LOOP('',(#8053,#8054,#8055,#8056));
#1493=EDGE_LOOP('',(#8057,#8058,#8059,#8060));
#1494=EDGE_LOOP('',(#8061,#8062,#8063,#8064));
#1495=EDGE_LOOP('',(#8065,#8066,#8067,#8068));
#1496=EDGE_LOOP('',(#8069,#8070,#8071,#8072));
#1497=EDGE_LOOP('',(#8073,#8074,#8075,#8076));
#1498=EDGE_LOOP('',(#8077,#8078,#8079,#8080));
#1499=EDGE_LOOP('',(#8081,#8082,#8083,#8084));
#1500=EDGE_LOOP('',(#8085,#8086,#8087));
#1501=EDGE_LOOP('',(#8088,#8089,#8090,#8091));
#1502=EDGE_LOOP('',(#8092,#8093,#8094,#8095));
#1503=EDGE_LOOP('',(#8096,#8097,#8098,#8099));
#1504=EDGE_LOOP('',(#8100,#8101,#8102,#8103));
#1505=EDGE_LOOP('',(#8104,#8105,#8106));
#1506=EDGE_LOOP('',(#8107,#8108,#8109,#8110));
#1507=EDGE_LOOP('',(#8111,#8112,#8113,#8114,#8115,#8116));
#1508=EDGE_LOOP('',(#8117));
#1509=EDGE_LOOP('',(#8118));
#1510=EDGE_LOOP('',(#8119,#8120,#8121,#8122));
#1511=EDGE_LOOP('',(#8123,#8124,#8125,#8126));
#1512=EDGE_LOOP('',(#8127,#8128,#8129,#8130));
#1513=EDGE_LOOP('',(#8131,#8132,#8133));
#1514=EDGE_LOOP('',(#8134,#8135,#8136));
#1515=EDGE_LOOP('',(#8137,#8138,#8139,#8140));
#1516=EDGE_LOOP('',(#8141,#8142,#8143));
#1517=EDGE_LOOP('',(#8144,#8145,#8146));
#1518=EDGE_LOOP('',(#8147,#8148,#8149,#8150));
#1519=EDGE_LOOP('',(#8151,#8152,#8153,#8154));
#1520=EDGE_LOOP('',(#8155,#8156,#8157,#8158));
#1521=EDGE_LOOP('',(#8159,#8160,#8161,#8162));
#1522=EDGE_LOOP('',(#8163,#8164,#8165));
#1523=EDGE_LOOP('',(#8166,#8167,#8168));
#1524=EDGE_LOOP('',(#8169,#8170,#8171,#8172));
#1525=EDGE_LOOP('',(#8173,#8174,#8175));
#1526=EDGE_LOOP('',(#8176,#8177,#8178));
#1527=EDGE_LOOP('',(#8179,#8180,#8181,#8182));
#1528=EDGE_LOOP('',(#8183,#8184,#8185,#8186));
#1529=EDGE_LOOP('',(#8187,#8188,#8189,#8190));
#1530=EDGE_LOOP('',(#8191,#8192,#8193,#8194));
#1531=EDGE_LOOP('',(#8195));
#1532=EDGE_LOOP('',(#8196));
#1533=EDGE_LOOP('',(#8197));
#1534=EDGE_LOOP('',(#8198));
#1535=EDGE_LOOP('',(#8199));
#1536=EDGE_LOOP('',(#8200));
#1537=EDGE_LOOP('',(#8201));
#1538=EDGE_LOOP('',(#8202));
#1539=EDGE_LOOP('',(#8203));
#1540=EDGE_LOOP('',(#8204));
#1541=EDGE_LOOP('',(#8205));
#1542=EDGE_LOOP('',(#8206));
#1543=EDGE_LOOP('',(#8207));
#1544=EDGE_LOOP('',(#8208));
#1545=EDGE_LOOP('',(#8209));
#1546=EDGE_LOOP('',(#8210));
#1547=EDGE_LOOP('',(#8211,#8212,#8213,#8214));
#1548=EDGE_LOOP('',(#8215,#8216,#8217,#8218));
#1549=EDGE_LOOP('',(#8219,#8220,#8221,#8222));
#1550=EDGE_LOOP('',(#8223,#8224,#8225));
#1551=EDGE_LOOP('',(#8226,#8227,#8228));
#1552=EDGE_LOOP('',(#8229,#8230,#8231,#8232));
#1553=EDGE_LOOP('',(#8233,#8234,#8235,#8236));
#1554=EDGE_LOOP('',(#8237,#8238,#8239,#8240));
#1555=EDGE_LOOP('',(#8241,#8242,#8243,#8244));
#1556=EDGE_LOOP('',(#8245,#8246,#8247,#8248));
#1557=EDGE_LOOP('',(#8249,#8250,#8251,#8252));
#1558=EDGE_LOOP('',(#8253,#8254,#8255,#8256));
#1559=EDGE_LOOP('',(#8257,#8258,#8259,#8260));
#1560=EDGE_LOOP('',(#8261,#8262,#8263,#8264));
#1561=EDGE_LOOP('',(#8265,#8266,#8267,#8268));
#1562=EDGE_LOOP('',(#8269,#8270,#8271,#8272));
#1563=EDGE_LOOP('',(#8273,#8274,#8275,#8276));
#1564=EDGE_LOOP('',(#8277,#8278,#8279,#8280));
#1565=EDGE_LOOP('',(#8281,#8282,#8283));
#1566=EDGE_LOOP('',(#8284,#8285,#8286));
#1567=EDGE_LOOP('',(#8287,#8288,#8289));
#1568=EDGE_LOOP('',(#8290,#8291,#8292,#8293));
#1569=EDGE_LOOP('',(#8294,#8295,#8296,#8297));
#1570=EDGE_LOOP('',(#8298,#8299,#8300,#8301));
#1571=EDGE_LOOP('',(#8302,#8303,#8304,#8305));
#1572=EDGE_LOOP('',(#8306,#8307,#8308,#8309));
#1573=EDGE_LOOP('',(#8310,#8311,#8312,#8313));
#1574=EDGE_LOOP('',(#8314,#8315,#8316,#8317));
#1575=EDGE_LOOP('',(#8318,#8319,#8320,#8321));
#1576=EDGE_LOOP('',(#8322,#8323,#8324,#8325));
#1577=EDGE_LOOP('',(#8326,#8327,#8328,#8329));
#1578=EDGE_LOOP('',(#8330,#8331,#8332));
#1579=EDGE_LOOP('',(#8333,#8334,#8335));
#1580=EDGE_LOOP('',(#8336,#8337,#8338,#8339));
#1581=EDGE_LOOP('',(#8340,#8341,#8342,#8343));
#1582=EDGE_LOOP('',(#8344,#8345,#8346,#8347));
#1583=EDGE_LOOP('',(#8348,#8349,#8350,#8351));
#1584=EDGE_LOOP('',(#8352,#8353,#8354,#8355));
#1585=EDGE_LOOP('',(#8356,#8357,#8358,#8359));
#1586=EDGE_LOOP('',(#8360,#8361,#8362,#8363));
#1587=EDGE_LOOP('',(#8364,#8365,#8366));
#1588=EDGE_LOOP('',(#8367,#8368,#8369,#8370));
#1589=EDGE_LOOP('',(#8371,#8372,#8373,#8374));
#1590=EDGE_LOOP('',(#8375,#8376,#8377,#8378));
#1591=EDGE_LOOP('',(#8379,#8380,#8381,#8382));
#1592=EDGE_LOOP('',(#8383,#8384,#8385,#8386));
#1593=EDGE_LOOP('',(#8387,#8388,#8389,#8390));
#1594=EDGE_LOOP('',(#8391,#8392,#8393,#8394));
#1595=EDGE_LOOP('',(#8395,#8396,#8397,#8398));
#1596=EDGE_LOOP('',(#8399,#8400,#8401,#8402));
#1597=EDGE_LOOP('',(#8403,#8404,#8405,#8406));
#1598=EDGE_LOOP('',(#8407,#8408,#8409,#8410));
#1599=EDGE_LOOP('',(#8411,#8412,#8413,#8414));
#1600=EDGE_LOOP('',(#8415,#8416,#8417,#8418));
#1601=EDGE_LOOP('',(#8419,#8420,#8421,#8422));
#1602=EDGE_LOOP('',(#8423,#8424,#8425,#8426));
#1603=EDGE_LOOP('',(#8427,#8428,#8429));
#1604=EDGE_LOOP('',(#8430,#8431,#8432,#8433));
#1605=EDGE_LOOP('',(#8434,#8435,#8436,#8437));
#1606=EDGE_LOOP('',(#8438,#8439,#8440,#8441));
#1607=EDGE_LOOP('',(#8442,#8443,#8444,#8445));
#1608=EDGE_LOOP('',(#8446,#8447,#8448,#8449));
#1609=EDGE_LOOP('',(#8450,#8451,#8452));
#1610=EDGE_LOOP('',(#8453,#8454,#8455));
#1611=EDGE_LOOP('',(#8456,#8457,#8458));
#1612=EDGE_LOOP('',(#8459,#8460,#8461));
#1613=EDGE_LOOP('',(#8462,#8463,#8464,#8465));
#1614=EDGE_LOOP('',(#8466,#8467,#8468,#8469));
#1615=EDGE_LOOP('',(#8470,#8471,#8472,#8473));
#1616=EDGE_LOOP('',(#8474,#8475,#8476,#8477));
#1617=EDGE_LOOP('',(#8478,#8479,#8480,#8481));
#1618=EDGE_LOOP('',(#8482,#8483,#8484,#8485));
#1619=EDGE_LOOP('',(#8486,#8487,#8488,#8489));
#1620=EDGE_LOOP('',(#8490,#8491,#8492));
#1621=EDGE_LOOP('',(#8493,#8494,#8495));
#1622=EDGE_LOOP('',(#8496,#8497,#8498,#8499));
#1623=EDGE_LOOP('',(#8500,#8501,#8502,#8503));
#1624=EDGE_LOOP('',(#8504,#8505,#8506,#8507));
#1625=EDGE_LOOP('',(#8508,#8509,#8510,#8511));
#1626=EDGE_LOOP('',(#8512,#8513,#8514,#8515));
#1627=EDGE_LOOP('',(#8516,#8517,#8518));
#1628=EDGE_LOOP('',(#8519,#8520,#8521));
#1629=EDGE_LOOP('',(#8522,#8523,#8524,#8525));
#1630=EDGE_LOOP('',(#8526,#8527,#8528,#8529));
#1631=EDGE_LOOP('',(#8530,#8531,#8532,#8533));
#1632=EDGE_LOOP('',(#8534,#8535,#8536,#8537));
#1633=EDGE_LOOP('',(#8538,#8539,#8540,#8541));
#1634=EDGE_LOOP('',(#8542,#8543,#8544,#8545));
#1635=EDGE_LOOP('',(#8546,#8547,#8548,#8549));
#1636=EDGE_LOOP('',(#8550,#8551,#8552,#8553));
#1637=EDGE_LOOP('',(#8554,#8555,#8556,#8557,#8558));
#1638=EDGE_LOOP('',(#8559,#8560,#8561,#8562));
#1639=EDGE_LOOP('',(#8563,#8564,#8565,#8566));
#1640=EDGE_LOOP('',(#8567,#8568,#8569,#8570));
#1641=EDGE_LOOP('',(#8571,#8572,#8573,#8574));
#1642=EDGE_LOOP('',(#8575,#8576,#8577,#8578));
#1643=EDGE_LOOP('',(#8579,#8580,#8581,#8582));
#1644=EDGE_LOOP('',(#8583,#8584,#8585,#8586));
#1645=EDGE_LOOP('',(#8587,#8588,#8589));
#1646=EDGE_LOOP('',(#8590,#8591,#8592,#8593));
#1647=EDGE_LOOP('',(#8594,#8595,#8596,#8597));
#1648=EDGE_LOOP('',(#8598,#8599,#8600,#8601));
#1649=EDGE_LOOP('',(#8602,#8603,#8604,#8605));
#1650=EDGE_LOOP('',(#8606,#8607,#8608,#8609));
#1651=EDGE_LOOP('',(#8610,#8611,#8612));
#1652=EDGE_LOOP('',(#8613,#8614,#8615,#8616));
#1653=EDGE_LOOP('',(#8617,#8618,#8619,#8620));
#1654=EDGE_LOOP('',(#8621,#8622,#8623,#8624));
#1655=EDGE_LOOP('',(#8625,#8626,#8627,#8628));
#1656=EDGE_LOOP('',(#8629,#8630,#8631,#8632));
#1657=EDGE_LOOP('',(#8633,#8634,#8635));
#1658=EDGE_LOOP('',(#8636,#8637,#8638,#8639));
#1659=EDGE_LOOP('',(#8640,#8641,#8642,#8643));
#1660=EDGE_LOOP('',(#8644,#8645,#8646,#8647,#8648));
#1661=EDGE_LOOP('',(#8649,#8650,#8651,#8652,#8653));
#1662=EDGE_LOOP('',(#8654,#8655,#8656,#8657,#8658));
#1663=EDGE_LOOP('',(#8659,#8660,#8661,#8662));
#1664=EDGE_LOOP('',(#8663,#8664,#8665,#8666,#8667,#8668,#8669,#8670,#8671,
#8672,#8673,#8674,#8675,#8676,#8677,#8678,#8679,#8680,#8681,#8682,#8683,
#8684,#8685,#8686));
#1665=EDGE_LOOP('',(#8687,#8688,#8689,#8690,#8691,#8692,#8693,#8694,#8695,
#8696,#8697,#8698));
#1666=EDGE_LOOP('',(#8699,#8700,#8701,#8702));
#1667=EDGE_LOOP('',(#8703,#8704,#8705,#8706));
#1668=EDGE_LOOP('',(#8707,#8708,#8709,#8710));
#1669=EDGE_LOOP('',(#8711,#8712,#8713,#8714));
#1670=EDGE_LOOP('',(#8715,#8716,#8717,#8718));
#1671=EDGE_LOOP('',(#8719,#8720,#8721,#8722));
#1672=EDGE_LOOP('',(#8723,#8724,#8725,#8726));
#1673=EDGE_LOOP('',(#8727,#8728,#8729,#8730));
#1674=EDGE_LOOP('',(#8731,#8732,#8733,#8734));
#1675=EDGE_LOOP('',(#8735,#8736,#8737,#8738,#8739,#8740));
#1676=EDGE_LOOP('',(#8741,#8742,#8743,#8744,#8745));
#1677=EDGE_LOOP('',(#8746,#8747,#8748,#8749));
#1678=EDGE_LOOP('',(#8750,#8751,#8752,#8753));
#1679=EDGE_LOOP('',(#8754,#8755,#8756,#8757));
#1680=EDGE_LOOP('',(#8758,#8759,#8760,#8761));
#1681=EDGE_LOOP('',(#8762,#8763,#8764,#8765));
#1682=EDGE_LOOP('',(#8766,#8767,#8768,#8769));
#1683=EDGE_LOOP('',(#8770,#8771,#8772,#8773));
#1684=EDGE_LOOP('',(#8774,#8775,#8776,#8777));
#1685=EDGE_LOOP('',(#8778,#8779,#8780,#8781));
#1686=EDGE_LOOP('',(#8782,#8783,#8784,#8785));
#1687=EDGE_LOOP('',(#8786,#8787,#8788,#8789,#8790,#8791,#8792,#8793,#8794,
#8795,#8796,#8797,#8798,#8799,#8800,#8801,#8802,#8803,#8804,#8805,#8806,
#8807,#8808,#8809,#8810,#8811,#8812,#8813,#8814,#8815,#8816,#8817,#8818,
#8819,#8820,#8821,#8822,#8823,#8824,#8825,#8826,#8827,#8828,#8829,#8830,
#8831,#8832,#8833,#8834,#8835,#8836,#8837,#8838,#8839,#8840,#8841,#8842,
#8843,#8844,#8845,#8846));
#1688=EDGE_LOOP('',(#8847,#8848,#8849,#8850));
#1689=EDGE_LOOP('',(#8851));
#1690=EDGE_LOOP('',(#8852,#8853,#8854,#8855));
#1691=EDGE_LOOP('',(#8856));
#1692=EDGE_LOOP('',(#8857));
#1693=EDGE_LOOP('',(#8858));
#1694=EDGE_LOOP('',(#8859));
#1695=EDGE_LOOP('',(#8860,#8861,#8862,#8863));
#1696=EDGE_LOOP('',(#8864,#8865,#8866,#8867,#8868,#8869));
#1697=EDGE_LOOP('',(#8870,#8871,#8872,#8873));
#1698=EDGE_LOOP('',(#8874,#8875,#8876,#8877));
#1699=EDGE_LOOP('',(#8878,#8879,#8880,#8881,#8882,#8883));
#1700=EDGE_LOOP('',(#8884,#8885,#8886,#8887));
#1701=EDGE_LOOP('',(#8888,#8889,#8890,#8891));
#1702=EDGE_LOOP('',(#8892,#8893,#8894,#8895,#8896,#8897));
#1703=EDGE_LOOP('',(#8898,#8899,#8900,#8901));
#1704=EDGE_LOOP('',(#8902,#8903,#8904,#8905));
#1705=EDGE_LOOP('',(#8906,#8907,#8908,#8909,#8910,#8911));
#1706=EDGE_LOOP('',(#8912,#8913,#8914,#8915));
#1707=EDGE_LOOP('',(#8916,#8917,#8918,#8919,#8920,#8921));
#1708=EDGE_LOOP('',(#8922,#8923,#8924,#8925));
#1709=EDGE_LOOP('',(#8926,#8927,#8928,#8929));
#1710=EDGE_LOOP('',(#8930,#8931,#8932,#8933,#8934,#8935));
#1711=EDGE_LOOP('',(#8936,#8937,#8938,#8939));
#1712=EDGE_LOOP('',(#8940,#8941,#8942,#8943,#8944,#8945));
#1713=EDGE_LOOP('',(#8946,#8947,#8948,#8949));
#1714=EDGE_LOOP('',(#8950,#8951,#8952,#8953));
#1715=EDGE_LOOP('',(#8954,#8955,#8956,#8957,#8958,#8959));
#1716=EDGE_LOOP('',(#8960,#8961,#8962,#8963));
#1717=EDGE_LOOP('',(#8964,#8965,#8966,#8967,#8968,#8969));
#1718=EDGE_LOOP('',(#8970,#8971,#8972,#8973));
#1719=EDGE_LOOP('',(#8974,#8975,#8976,#8977));
#1720=EDGE_LOOP('',(#8978,#8979,#8980,#8981,#8982,#8983));
#1721=EDGE_LOOP('',(#8984,#8985,#8986,#8987));
#1722=EDGE_LOOP('',(#8988,#8989,#8990,#8991,#8992,#8993));
#1723=EDGE_LOOP('',(#8994,#8995,#8996,#8997));
#1724=EDGE_LOOP('',(#8998,#8999,#9000,#9001));
#1725=EDGE_LOOP('',(#9002,#9003,#9004,#9005,#9006,#9007));
#1726=EDGE_LOOP('',(#9008,#9009,#9010,#9011));
#1727=EDGE_LOOP('',(#9012,#9013,#9014,#9015,#9016,#9017));
#1728=EDGE_LOOP('',(#9018,#9019,#9020,#9021));
#1729=EDGE_LOOP('',(#9022,#9023,#9024,#9025));
#1730=EDGE_LOOP('',(#9026,#9027,#9028,#9029,#9030,#9031));
#1731=EDGE_LOOP('',(#9032,#9033,#9034,#9035));
#1732=EDGE_LOOP('',(#9036,#9037,#9038,#9039,#9040,#9041));
#1733=EDGE_LOOP('',(#9042,#9043,#9044,#9045));
#1734=EDGE_LOOP('',(#9046,#9047,#9048,#9049));
#1735=EDGE_LOOP('',(#9050,#9051,#9052,#9053,#9054,#9055));
#1736=EDGE_LOOP('',(#9056,#9057,#9058,#9059));
#1737=EDGE_LOOP('',(#9060,#9061,#9062,#9063,#9064,#9065));
#1738=EDGE_LOOP('',(#9066,#9067,#9068,#9069));
#1739=EDGE_LOOP('',(#9070,#9071,#9072,#9073));
#1740=EDGE_LOOP('',(#9074,#9075,#9076,#9077,#9078,#9079));
#1741=EDGE_LOOP('',(#9080,#9081,#9082,#9083));
#1742=EDGE_LOOP('',(#9084,#9085,#9086,#9087,#9088,#9089));
#1743=EDGE_LOOP('',(#9090,#9091,#9092,#9093));
#1744=EDGE_LOOP('',(#9094,#9095,#9096,#9097));
#1745=EDGE_LOOP('',(#9098,#9099,#9100,#9101,#9102,#9103));
#1746=EDGE_LOOP('',(#9104,#9105,#9106,#9107));
#1747=EDGE_LOOP('',(#9108,#9109,#9110,#9111));
#1748=EDGE_LOOP('',(#9112,#9113,#9114,#9115));
#1749=EDGE_LOOP('',(#9116,#9117,#9118,#9119));
#1750=EDGE_LOOP('',(#9120,#9121,#9122,#9123));
#1751=EDGE_LOOP('',(#9124,#9125,#9126,#9127));
#1752=EDGE_LOOP('',(#9128,#9129,#9130,#9131));
#1753=EDGE_LOOP('',(#9132,#9133,#9134,#9135));
#1754=EDGE_LOOP('',(#9136,#9137,#9138,#9139));
#1755=EDGE_LOOP('',(#9140,#9141,#9142,#9143,#9144,#9145));
#1756=EDGE_LOOP('',(#9146,#9147,#9148,#9149,#9150,#9151));
#1757=EDGE_LOOP('',(#9152,#9153,#9154,#9155,#9156,#9157));
#1758=EDGE_LOOP('',(#9158,#9159,#9160,#9161,#9162,#9163));
#1759=EDGE_LOOP('',(#9164,#9165,#9166,#9167,#9168,#9169));
#1760=EDGE_LOOP('',(#9170,#9171,#9172,#9173,#9174,#9175));
#1761=EDGE_LOOP('',(#9176,#9177,#9178,#9179,#9180,#9181));
#1762=EDGE_LOOP('',(#9182,#9183,#9184,#9185,#9186,#9187));
#1763=EDGE_LOOP('',(#9188,#9189,#9190,#9191,#9192,#9193,#9194,#9195));
#1764=EDGE_LOOP('',(#9196,#9197,#9198,#9199,#9200,#9201));
#1765=EDGE_LOOP('',(#9202));
#1766=EDGE_LOOP('',(#9203));
#1767=EDGE_LOOP('',(#9204,#9205,#9206,#9207));
#1768=EDGE_LOOP('',(#9208,#9209,#9210,#9211));
#1769=EDGE_LOOP('',(#9212,#9213,#9214,#9215));
#1770=EDGE_LOOP('',(#9216,#9217,#9218,#9219,#9220));
#1771=EDGE_LOOP('',(#9221,#9222,#9223,#9224,#9225));
#1772=EDGE_LOOP('',(#9226,#9227,#9228,#9229));
#1773=EDGE_LOOP('',(#9230,#9231,#9232,#9233));
#1774=EDGE_LOOP('',(#9234,#9235,#9236,#9237));
#1775=EDGE_LOOP('',(#9238,#9239,#9240,#9241));
#1776=EDGE_LOOP('',(#9242,#9243,#9244,#9245));
#1777=EDGE_LOOP('',(#9246,#9247,#9248,#9249));
#1778=EDGE_LOOP('',(#9250,#9251,#9252,#9253));
#1779=EDGE_LOOP('',(#9254,#9255,#9256,#9257));
#1780=EDGE_LOOP('',(#9258,#9259,#9260,#9261));
#1781=EDGE_LOOP('',(#9262,#9263,#9264,#9265));
#1782=EDGE_LOOP('',(#9266,#9267,#9268,#9269));
#1783=EDGE_LOOP('',(#9270,#9271,#9272,#9273));
#1784=EDGE_LOOP('',(#9274,#9275,#9276,#9277));
#1785=EDGE_LOOP('',(#9278,#9279,#9280,#9281,#9282,#9283));
#1786=EDGE_LOOP('',(#9284));
#1787=EDGE_LOOP('',(#9285));
#1788=EDGE_LOOP('',(#9286));
#1789=EDGE_LOOP('',(#9287));
#1790=EDGE_LOOP('',(#9288));
#1791=EDGE_LOOP('',(#9289));
#1792=EDGE_LOOP('',(#9290));
#1793=EDGE_LOOP('',(#9291));
#1794=EDGE_LOOP('',(#9292));
#1795=EDGE_LOOP('',(#9293));
#1796=EDGE_LOOP('',(#9294));
#1797=EDGE_LOOP('',(#9295));
#1798=EDGE_LOOP('',(#9296));
#1799=EDGE_LOOP('',(#9297));
#1800=EDGE_LOOP('',(#9298));
#1801=EDGE_LOOP('',(#9299));
#1802=EDGE_LOOP('',(#9300,#9301,#9302,#9303));
#1803=EDGE_LOOP('',(#9304,#9305,#9306,#9307));
#1804=EDGE_LOOP('',(#9308,#9309,#9310,#9311));
#1805=EDGE_LOOP('',(#9312,#9313,#9314,#9315));
#1806=EDGE_LOOP('',(#9316,#9317,#9318,#9319));
#1807=EDGE_LOOP('',(#9320,#9321,#9322,#9323));
#1808=EDGE_LOOP('',(#9324,#9325,#9326,#9327));
#1809=EDGE_LOOP('',(#9328,#9329,#9330,#9331));
#1810=EDGE_LOOP('',(#9332,#9333,#9334,#9335));
#1811=EDGE_LOOP('',(#9336,#9337,#9338,#9339));
#1812=EDGE_LOOP('',(#9340,#9341,#9342,#9343));
#1813=EDGE_LOOP('',(#9344,#9345,#9346,#9347));
#1814=EDGE_LOOP('',(#9348,#9349,#9350,#9351,#9352,#9353,#9354,#9355,#9356,
#9357,#9358,#9359));
#1815=EDGE_LOOP('',(#9360,#9361,#9362,#9363,#9364,#9365,#9366,#9367,#9368,
#9369,#9370,#9371));
#1816=EDGE_LOOP('',(#9372,#9373,#9374,#9375,#9376,#9377,#9378,#9379,#9380,
#9381,#9382,#9383));
#1817=EDGE_LOOP('',(#9384,#9385,#9386,#9387));
#1818=EDGE_LOOP('',(#9388,#9389,#9390,#9391));
#1819=EDGE_LOOP('',(#9392,#9393,#9394,#9395));
#1820=EDGE_LOOP('',(#9396,#9397,#9398,#9399));
#1821=EDGE_LOOP('',(#9400,#9401,#9402,#9403));
#1822=EDGE_LOOP('',(#9404,#9405,#9406,#9407));
#1823=EDGE_LOOP('',(#9408,#9409,#9410,#9411));
#1824=EDGE_LOOP('',(#9412,#9413,#9414,#9415));
#1825=EDGE_LOOP('',(#9416,#9417,#9418,#9419));
#1826=EDGE_LOOP('',(#9420,#9421,#9422,#9423));
#1827=EDGE_LOOP('',(#9424,#9425,#9426,#9427));
#1828=EDGE_LOOP('',(#9428,#9429,#9430,#9431));
#1829=EDGE_LOOP('',(#9432,#9433,#9434,#9435,#9436,#9437,#9438,#9439,#9440,
#9441,#9442,#9443));
#1830=EDGE_LOOP('',(#9444,#9445,#9446,#9447,#9448,#9449,#9450,#9451,#9452,
#9453,#9454,#9455));
#1831=EDGE_LOOP('',(#9456,#9457,#9458,#9459));
#1832=EDGE_LOOP('',(#9460,#9461,#9462,#9463));
#1833=EDGE_LOOP('',(#9464,#9465,#9466,#9467));
#1834=EDGE_LOOP('',(#9468,#9469,#9470,#9471));
#1835=EDGE_LOOP('',(#9472,#9473,#9474,#9475));
#1836=EDGE_LOOP('',(#9476,#9477,#9478,#9479));
#1837=EDGE_LOOP('',(#9480,#9481,#9482,#9483));
#1838=EDGE_LOOP('',(#9484,#9485,#9486,#9487));
#1839=EDGE_LOOP('',(#9488,#9489,#9490,#9491));
#1840=EDGE_LOOP('',(#9492,#9493,#9494,#9495));
#1841=EDGE_LOOP('',(#9496,#9497,#9498,#9499));
#1842=EDGE_LOOP('',(#9500,#9501,#9502,#9503));
#1843=EDGE_LOOP('',(#9504,#9505,#9506,#9507,#9508,#9509,#9510,#9511,#9512,
#9513,#9514,#9515));
#1844=EDGE_LOOP('',(#9516,#9517,#9518,#9519));
#1845=EDGE_LOOP('',(#9520,#9521,#9522,#9523));
#1846=EDGE_LOOP('',(#9524,#9525,#9526,#9527));
#1847=EDGE_LOOP('',(#9528,#9529,#9530,#9531));
#1848=EDGE_LOOP('',(#9532,#9533,#9534,#9535));
#1849=EDGE_LOOP('',(#9536,#9537,#9538,#9539));
#1850=EDGE_LOOP('',(#9540,#9541,#9542,#9543));
#1851=EDGE_LOOP('',(#9544,#9545,#9546,#9547));
#1852=EDGE_LOOP('',(#9548,#9549,#9550,#9551));
#1853=EDGE_LOOP('',(#9552,#9553,#9554,#9555));
#1854=EDGE_LOOP('',(#9556,#9557,#9558,#9559));
#1855=EDGE_LOOP('',(#9560,#9561,#9562,#9563));
#1856=EDGE_LOOP('',(#9564,#9565,#9566,#9567,#9568,#9569,#9570,#9571,#9572,
#9573,#9574,#9575));
#1857=EDGE_LOOP('',(#9576,#9577,#9578,#9579,#9580,#9581,#9582,#9583,#9584,
#9585,#9586,#9587));
#1858=EDGE_LOOP('',(#9588,#9589,#9590,#9591));
#1859=EDGE_LOOP('',(#9592,#9593,#9594,#9595));
#1860=EDGE_LOOP('',(#9596,#9597,#9598,#9599));
#1861=EDGE_LOOP('',(#9600,#9601,#9602,#9603));
#1862=EDGE_LOOP('',(#9604,#9605,#9606,#9607));
#1863=EDGE_LOOP('',(#9608,#9609,#9610,#9611));
#1864=EDGE_LOOP('',(#9612,#9613,#9614,#9615));
#1865=EDGE_LOOP('',(#9616,#9617,#9618,#9619));
#1866=EDGE_LOOP('',(#9620,#9621,#9622,#9623));
#1867=EDGE_LOOP('',(#9624,#9625,#9626,#9627));
#1868=EDGE_LOOP('',(#9628,#9629,#9630,#9631));
#1869=EDGE_LOOP('',(#9632,#9633,#9634,#9635));
#1870=EDGE_LOOP('',(#9636,#9637,#9638,#9639,#9640,#9641,#9642,#9643,#9644,
#9645,#9646,#9647));
#1871=EDGE_LOOP('',(#9648,#9649,#9650,#9651,#9652,#9653,#9654,#9655,#9656,
#9657,#9658,#9659));
#1872=EDGE_LOOP('',(#9660,#9661,#9662,#9663,#9664,#9665,#9666,#9667,#9668,
#9669,#9670,#9671));
#1873=EDGE_LOOP('',(#9672,#9673,#9674,#9675));
#1874=EDGE_LOOP('',(#9676,#9677,#9678,#9679));
#1875=EDGE_LOOP('',(#9680,#9681,#9682,#9683));
#1876=EDGE_LOOP('',(#9684,#9685,#9686,#9687));
#1877=EDGE_LOOP('',(#9688,#9689,#9690,#9691));
#1878=EDGE_LOOP('',(#9692,#9693,#9694,#9695));
#1879=EDGE_LOOP('',(#9696,#9697,#9698,#9699));
#1880=EDGE_LOOP('',(#9700,#9701,#9702,#9703));
#1881=EDGE_LOOP('',(#9704,#9705,#9706,#9707));
#1882=EDGE_LOOP('',(#9708,#9709,#9710,#9711));
#1883=EDGE_LOOP('',(#9712,#9713,#9714,#9715));
#1884=EDGE_LOOP('',(#9716,#9717,#9718,#9719));
#1885=EDGE_LOOP('',(#9720,#9721,#9722,#9723,#9724,#9725,#9726,#9727,#9728,
#9729,#9730,#9731));
#1886=EDGE_LOOP('',(#9732,#9733,#9734,#9735));
#1887=EDGE_LOOP('',(#9736,#9737,#9738,#9739));
#1888=EDGE_LOOP('',(#9740,#9741,#9742,#9743));
#1889=EDGE_LOOP('',(#9744,#9745,#9746,#9747));
#1890=EDGE_LOOP('',(#9748,#9749,#9750,#9751));
#1891=EDGE_LOOP('',(#9752,#9753,#9754,#9755));
#1892=EDGE_LOOP('',(#9756,#9757,#9758,#9759));
#1893=EDGE_LOOP('',(#9760,#9761,#9762,#9763));
#1894=EDGE_LOOP('',(#9764,#9765,#9766,#9767));
#1895=EDGE_LOOP('',(#9768,#9769,#9770,#9771));
#1896=EDGE_LOOP('',(#9772,#9773,#9774,#9775));
#1897=EDGE_LOOP('',(#9776,#9777,#9778,#9779));
#1898=EDGE_LOOP('',(#9780,#9781,#9782,#9783,#9784,#9785,#9786,#9787,#9788,
#9789,#9790,#9791));
#1899=EDGE_LOOP('',(#9792,#9793,#9794,#9795,#9796,#9797,#9798,#9799,#9800,
#9801,#9802,#9803));
#1900=EDGE_LOOP('',(#9804,#9805,#9806,#9807,#9808,#9809,#9810,#9811,#9812,
#9813,#9814,#9815));
#1901=EDGE_LOOP('',(#9816,#9817,#9818,#9819));
#1902=EDGE_LOOP('',(#9820,#9821,#9822,#9823));
#1903=EDGE_LOOP('',(#9824,#9825,#9826,#9827));
#1904=EDGE_LOOP('',(#9828,#9829,#9830,#9831));
#1905=EDGE_LOOP('',(#9832,#9833,#9834,#9835));
#1906=EDGE_LOOP('',(#9836,#9837,#9838,#9839));
#1907=EDGE_LOOP('',(#9840,#9841,#9842,#9843));
#1908=EDGE_LOOP('',(#9844,#9845,#9846,#9847));
#1909=EDGE_LOOP('',(#9848,#9849,#9850,#9851));
#1910=EDGE_LOOP('',(#9852,#9853,#9854,#9855));
#1911=EDGE_LOOP('',(#9856,#9857,#9858,#9859));
#1912=EDGE_LOOP('',(#9860,#9861,#9862,#9863));
#1913=EDGE_LOOP('',(#9864,#9865,#9866,#9867,#9868,#9869,#9870,#9871,#9872,
#9873,#9874,#9875));
#1914=EDGE_LOOP('',(#9876,#9877,#9878,#9879,#9880,#9881,#9882,#9883,#9884,
#9885,#9886,#9887));
#1915=EDGE_LOOP('',(#9888,#9889,#9890,#9891));
#1916=EDGE_LOOP('',(#9892,#9893,#9894,#9895));
#1917=EDGE_LOOP('',(#9896,#9897,#9898,#9899));
#1918=EDGE_LOOP('',(#9900,#9901,#9902,#9903));
#1919=EDGE_LOOP('',(#9904,#9905,#9906,#9907));
#1920=EDGE_LOOP('',(#9908,#9909,#9910,#9911));
#1921=EDGE_LOOP('',(#9912,#9913,#9914,#9915));
#1922=EDGE_LOOP('',(#9916,#9917,#9918,#9919));
#1923=EDGE_LOOP('',(#9920,#9921,#9922,#9923));
#1924=EDGE_LOOP('',(#9924,#9925,#9926,#9927));
#1925=EDGE_LOOP('',(#9928,#9929,#9930,#9931));
#1926=EDGE_LOOP('',(#9932,#9933,#9934,#9935));
#1927=EDGE_LOOP('',(#9936,#9937,#9938,#9939,#9940,#9941,#9942,#9943,#9944,
#9945,#9946,#9947));
#1928=EDGE_LOOP('',(#9948,#9949,#9950,#9951,#9952,#9953,#9954,#9955,#9956,
#9957,#9958,#9959));
#1929=EDGE_LOOP('',(#9960,#9961,#9962,#9963));
#1930=EDGE_LOOP('',(#9964,#9965,#9966,#9967));
#1931=EDGE_LOOP('',(#9968,#9969,#9970,#9971));
#1932=EDGE_LOOP('',(#9972,#9973,#9974,#9975));
#1933=EDGE_LOOP('',(#9976,#9977,#9978,#9979));
#1934=EDGE_LOOP('',(#9980,#9981,#9982,#9983));
#1935=EDGE_LOOP('',(#9984,#9985,#9986,#9987));
#1936=EDGE_LOOP('',(#9988,#9989,#9990,#9991));
#1937=EDGE_LOOP('',(#9992,#9993,#9994,#9995));
#1938=EDGE_LOOP('',(#9996,#9997,#9998,#9999));
#1939=EDGE_LOOP('',(#10000,#10001,#10002,#10003));
#1940=EDGE_LOOP('',(#10004,#10005,#10006,#10007));
#1941=EDGE_LOOP('',(#10008,#10009,#10010,#10011,#10012,#10013,#10014,#10015,
#10016,#10017,#10018,#10019));
#1942=EDGE_LOOP('',(#10020,#10021,#10022,#10023));
#1943=EDGE_LOOP('',(#10024,#10025,#10026,#10027));
#1944=EDGE_LOOP('',(#10028,#10029,#10030,#10031));
#1945=EDGE_LOOP('',(#10032,#10033,#10034,#10035));
#1946=EDGE_LOOP('',(#10036,#10037,#10038,#10039));
#1947=EDGE_LOOP('',(#10040,#10041,#10042,#10043));
#1948=EDGE_LOOP('',(#10044,#10045,#10046,#10047));
#1949=EDGE_LOOP('',(#10048,#10049,#10050,#10051));
#1950=EDGE_LOOP('',(#10052,#10053,#10054,#10055));
#1951=EDGE_LOOP('',(#10056,#10057,#10058,#10059,#10060,#10061,#10062,#10063,
#10064));
#1952=EDGE_LOOP('',(#10065,#10066,#10067,#10068,#10069,#10070,#10071,#10072,
#10073));
#1953=EDGE_LOOP('',(#10074,#10075,#10076,#10077));
#1954=EDGE_LOOP('',(#10078,#10079,#10080,#10081));
#1955=EDGE_LOOP('',(#10082,#10083,#10084,#10085));
#1956=EDGE_LOOP('',(#10086,#10087,#10088,#10089));
#1957=EDGE_LOOP('',(#10090,#10091,#10092,#10093));
#1958=EDGE_LOOP('',(#10094,#10095,#10096,#10097));
#1959=EDGE_LOOP('',(#10098,#10099,#10100,#10101));
#1960=EDGE_LOOP('',(#10102,#10103,#10104,#10105));
#1961=EDGE_LOOP('',(#10106,#10107,#10108,#10109));
#1962=EDGE_LOOP('',(#10110,#10111,#10112,#10113,#10114,#10115,#10116,#10117,
#10118));
#1963=EDGE_LOOP('',(#10119,#10120,#10121,#10122,#10123,#10124,#10125,#10126,
#10127));
#1964=EDGE_LOOP('',(#10128,#10129,#10130,#10131));
#1965=EDGE_LOOP('',(#10132,#10133,#10134,#10135));
#1966=EDGE_LOOP('',(#10136,#10137,#10138,#10139));
#1967=EDGE_LOOP('',(#10140,#10141,#10142,#10143));
#1968=EDGE_LOOP('',(#10144,#10145,#10146,#10147));
#1969=EDGE_LOOP('',(#10148,#10149,#10150,#10151));
#1970=EDGE_LOOP('',(#10152,#10153,#10154,#10155));
#1971=EDGE_LOOP('',(#10156,#10157,#10158,#10159));
#1972=EDGE_LOOP('',(#10160,#10161,#10162,#10163));
#1973=EDGE_LOOP('',(#10164,#10165,#10166,#10167,#10168,#10169,#10170,#10171,
#10172));
#1974=EDGE_LOOP('',(#10173,#10174,#10175,#10176,#10177,#10178,#10179,#10180,
#10181));
#1975=EDGE_LOOP('',(#10182,#10183,#10184,#10185));
#1976=EDGE_LOOP('',(#10186,#10187,#10188,#10189));
#1977=EDGE_LOOP('',(#10190,#10191,#10192,#10193));
#1978=EDGE_LOOP('',(#10194,#10195,#10196,#10197));
#1979=EDGE_LOOP('',(#10198,#10199,#10200,#10201));
#1980=EDGE_LOOP('',(#10202,#10203,#10204,#10205));
#1981=EDGE_LOOP('',(#10206,#10207,#10208,#10209));
#1982=EDGE_LOOP('',(#10210,#10211,#10212,#10213));
#1983=EDGE_LOOP('',(#10214,#10215,#10216,#10217));
#1984=EDGE_LOOP('',(#10218,#10219,#10220,#10221,#10222,#10223,#10224,#10225,
#10226));
#1985=EDGE_LOOP('',(#10227,#10228,#10229,#10230,#10231,#10232,#10233,#10234,
#10235));
#1986=EDGE_LOOP('',(#10236,#10237,#10238,#10239,#10240,#10241,#10242,#10243,
#10244));
#1987=EDGE_LOOP('',(#10245,#10246,#10247,#10248));
#1988=EDGE_LOOP('',(#10249,#10250,#10251,#10252));
#1989=EDGE_LOOP('',(#10253,#10254,#10255,#10256));
#1990=EDGE_LOOP('',(#10257,#10258,#10259,#10260));
#1991=EDGE_LOOP('',(#10261,#10262,#10263,#10264));
#1992=EDGE_LOOP('',(#10265,#10266,#10267,#10268));
#1993=EDGE_LOOP('',(#10269,#10270,#10271,#10272));
#1994=EDGE_LOOP('',(#10273,#10274,#10275,#10276));
#1995=EDGE_LOOP('',(#10277,#10278,#10279,#10280));
#1996=EDGE_LOOP('',(#10281,#10282,#10283,#10284,#10285,#10286,#10287,#10288,
#10289));
#1997=EDGE_LOOP('',(#10290,#10291,#10292,#10293));
#1998=EDGE_LOOP('',(#10294,#10295,#10296,#10297));
#1999=EDGE_LOOP('',(#10298,#10299,#10300,#10301));
#2000=EDGE_LOOP('',(#10302,#10303,#10304,#10305));
#2001=EDGE_LOOP('',(#10306,#10307,#10308,#10309));
#2002=EDGE_LOOP('',(#10310,#10311,#10312,#10313));
#2003=EDGE_LOOP('',(#10314,#10315,#10316,#10317));
#2004=EDGE_LOOP('',(#10318,#10319,#10320,#10321));
#2005=EDGE_LOOP('',(#10322,#10323,#10324,#10325));
#2006=EDGE_LOOP('',(#10326,#10327,#10328,#10329,#10330,#10331,#10332,#10333,
#10334));
#2007=EDGE_LOOP('',(#10335,#10336,#10337,#10338,#10339,#10340,#10341,#10342,
#10343));
#2008=EDGE_LOOP('',(#10344,#10345,#10346,#10347,#10348,#10349,#10350,#10351,
#10352));
#2009=EDGE_LOOP('',(#10353,#10354,#10355,#10356));
#2010=EDGE_LOOP('',(#10357,#10358,#10359,#10360));
#2011=EDGE_LOOP('',(#10361,#10362,#10363,#10364));
#2012=EDGE_LOOP('',(#10365,#10366,#10367,#10368));
#2013=EDGE_LOOP('',(#10369,#10370,#10371,#10372));
#2014=EDGE_LOOP('',(#10373,#10374,#10375,#10376));
#2015=EDGE_LOOP('',(#10377,#10378,#10379,#10380));
#2016=EDGE_LOOP('',(#10381,#10382,#10383,#10384));
#2017=EDGE_LOOP('',(#10385,#10386,#10387,#10388));
#2018=EDGE_LOOP('',(#10389,#10390,#10391,#10392,#10393,#10394,#10395,#10396,
#10397));
#2019=EDGE_LOOP('',(#10398,#10399,#10400,#10401,#10402,#10403,#10404,#10405,
#10406));
#2020=EDGE_LOOP('',(#10407,#10408,#10409,#10410));
#2021=EDGE_LOOP('',(#10411,#10412,#10413,#10414));
#2022=EDGE_LOOP('',(#10415,#10416,#10417,#10418));
#2023=EDGE_LOOP('',(#10419,#10420,#10421,#10422));
#2024=EDGE_LOOP('',(#10423,#10424,#10425,#10426));
#2025=EDGE_LOOP('',(#10427,#10428,#10429,#10430));
#2026=EDGE_LOOP('',(#10431,#10432,#10433,#10434));
#2027=EDGE_LOOP('',(#10435,#10436,#10437,#10438));
#2028=EDGE_LOOP('',(#10439,#10440,#10441,#10442));
#2029=EDGE_LOOP('',(#10443,#10444,#10445,#10446,#10447,#10448,#10449,#10450,
#10451));
#2030=EDGE_LOOP('',(#10452,#10453,#10454,#10455));
#2031=EDGE_LOOP('',(#10456,#10457,#10458,#10459));
#2032=EDGE_LOOP('',(#10460,#10461,#10462,#10463));
#2033=EDGE_LOOP('',(#10464,#10465,#10466,#10467));
#2034=EDGE_LOOP('',(#10468,#10469,#10470,#10471));
#2035=EDGE_LOOP('',(#10472,#10473,#10474,#10475));
#2036=EDGE_LOOP('',(#10476,#10477,#10478,#10479));
#2037=EDGE_LOOP('',(#10480,#10481,#10482,#10483));
#2038=EDGE_LOOP('',(#10484,#10485,#10486,#10487));
#2039=EDGE_LOOP('',(#10488,#10489,#10490,#10491,#10492,#10493,#10494,#10495,
#10496));
#2040=EDGE_LOOP('',(#10497,#10498,#10499,#10500,#10501,#10502,#10503,#10504,
#10505));
#2041=EDGE_LOOP('',(#10506,#10507,#10508,#10509,#10510,#10511,#10512,#10513,
#10514));
#2042=EDGE_LOOP('',(#10515,#10516,#10517,#10518));
#2043=EDGE_LOOP('',(#10519,#10520,#10521,#10522));
#2044=EDGE_LOOP('',(#10523,#10524,#10525,#10526));
#2045=EDGE_LOOP('',(#10527,#10528,#10529,#10530));
#2046=EDGE_LOOP('',(#10531,#10532,#10533,#10534));
#2047=EDGE_LOOP('',(#10535,#10536,#10537,#10538));
#2048=EDGE_LOOP('',(#10539,#10540,#10541,#10542));
#2049=EDGE_LOOP('',(#10543,#10544,#10545,#10546));
#2050=EDGE_LOOP('',(#10547,#10548,#10549,#10550));
#2051=EDGE_LOOP('',(#10551,#10552,#10553,#10554,#10555,#10556,#10557,#10558,
#10559));
#2052=EDGE_LOOP('',(#10560,#10561,#10562,#10563));
#2053=EDGE_LOOP('',(#10564,#10565,#10566,#10567));
#2054=EDGE_LOOP('',(#10568,#10569,#10570,#10571));
#2055=EDGE_LOOP('',(#10572,#10573,#10574,#10575));
#2056=EDGE_LOOP('',(#10576,#10577,#10578,#10579));
#2057=EDGE_LOOP('',(#10580,#10581,#10582,#10583));
#2058=EDGE_LOOP('',(#10584,#10585,#10586,#10587));
#2059=EDGE_LOOP('',(#10588,#10589,#10590,#10591));
#2060=EDGE_LOOP('',(#10592,#10593,#10594,#10595,#10596,#10597,#10598,#10599));
#2061=EDGE_LOOP('',(#10600,#10601,#10602,#10603));
#2062=EDGE_LOOP('',(#10604,#10605,#10606,#10607));
#2063=EDGE_LOOP('',(#10608,#10609,#10610,#10611));
#2064=EDGE_LOOP('',(#10612,#10613,#10614,#10615));
#2065=EDGE_LOOP('',(#10616,#10617,#10618,#10619,#10620,#10621,#10622,#10623));
#2066=EDGE_LOOP('',(#10624,#10625,#10626,#10627));
#2067=EDGE_LOOP('',(#10628,#10629,#10630,#10631));
#2068=EDGE_LOOP('',(#10632,#10633,#10634,#10635));
#2069=EDGE_LOOP('',(#10636,#10637,#10638,#10639));
#2070=EDGE_LOOP('',(#10640,#10641,#10642,#10643));
#2071=EDGE_LOOP('',(#10644,#10645,#10646,#10647));
#2072=EDGE_LOOP('',(#10648,#10649,#10650,#10651));
#2073=EDGE_LOOP('',(#10652,#10653,#10654,#10655));
#2074=EDGE_LOOP('',(#10656,#10657,#10658,#10659));
#2075=EDGE_LOOP('',(#10660,#10661,#10662,#10663));
#2076=EDGE_LOOP('',(#10664,#10665,#10666,#10667));
#2077=EDGE_LOOP('',(#10668,#10669,#10670,#10671));
#2078=EDGE_LOOP('',(#10672,#10673,#10674,#10675));
#2079=EDGE_LOOP('',(#10676,#10677,#10678,#10679));
#2080=EDGE_LOOP('',(#10680,#10681,#10682,#10683));
#2081=EDGE_LOOP('',(#10684,#10685,#10686,#10687));
#2082=EDGE_LOOP('',(#10688,#10689,#10690,#10691));
#2083=EDGE_LOOP('',(#10692,#10693,#10694,#10695));
#2084=EDGE_LOOP('',(#10696,#10697,#10698,#10699));
#2085=EDGE_LOOP('',(#10700,#10701,#10702,#10703));
#2086=EDGE_LOOP('',(#10704,#10705,#10706,#10707));
#2087=EDGE_LOOP('',(#10708,#10709,#10710,#10711));
#2088=EDGE_LOOP('',(#10712,#10713,#10714,#10715));
#2089=EDGE_LOOP('',(#10716,#10717,#10718,#10719));
#2090=EDGE_LOOP('',(#10720,#10721,#10722,#10723));
#2091=EDGE_LOOP('',(#10724,#10725,#10726,#10727));
#2092=EDGE_LOOP('',(#10728,#10729,#10730,#10731));
#2093=EDGE_LOOP('',(#10732,#10733,#10734,#10735));
#2094=EDGE_LOOP('',(#10736));
#2095=EDGE_LOOP('',(#10737));
#2096=EDGE_LOOP('',(#10738,#10739,#10740,#10741));
#2097=EDGE_LOOP('',(#10742,#10743,#10744,#10745));
#2098=EDGE_LOOP('',(#10746,#10747,#10748,#10749));
#2099=EDGE_LOOP('',(#10750,#10751,#10752,#10753));
#2100=EDGE_LOOP('',(#10754,#10755,#10756,#10757));
#2101=EDGE_LOOP('',(#10758,#10759,#10760,#10761));
#2102=EDGE_LOOP('',(#10762));
#2103=EDGE_LOOP('',(#10763));
#2104=EDGE_LOOP('',(#10764,#10765,#10766,#10767,#10768,#10769,#10770,#10771,
#10772,#10773,#10774,#10775));
#2105=EDGE_LOOP('',(#10776,#10777,#10778,#10779,#10780,#10781,#10782,#10783,
#10784,#10785,#10786,#10787));
#2106=EDGE_LOOP('',(#10788,#10789,#10790,#10791));
#2107=EDGE_LOOP('',(#10792,#10793,#10794,#10795));
#2108=EDGE_LOOP('',(#10796,#10797,#10798,#10799));
#2109=EDGE_LOOP('',(#10800));
#2110=EDGE_LOOP('',(#10801));
#2111=EDGE_LOOP('',(#10802,#10803,#10804,#10805));
#2112=EDGE_LOOP('',(#10806,#10807,#10808,#10809));
#2113=EDGE_LOOP('',(#10810,#10811,#10812,#10813));
#2114=EDGE_LOOP('',(#10814));
#2115=EDGE_LOOP('',(#10815));
#2116=EDGE_LOOP('',(#10816,#10817,#10818,#10819));
#2117=EDGE_LOOP('',(#10820,#10821,#10822,#10823));
#2118=EDGE_LOOP('',(#10824,#10825,#10826,#10827));
#2119=EDGE_LOOP('',(#10828,#10829,#10830,#10831));
#2120=EDGE_LOOP('',(#10832,#10833,#10834,#10835));
#2121=EDGE_LOOP('',(#10836,#10837,#10838,#10839,#10840,#10841,#10842,#10843,
#10844));
#2122=EDGE_LOOP('',(#10845,#10846,#10847,#10848,#10849,#10850,#10851,#10852,
#10853));
#2123=EDGE_LOOP('',(#10854,#10855,#10856,#10857));
#2124=EDGE_LOOP('',(#10858,#10859,#10860,#10861));
#2125=EDGE_LOOP('',(#10862,#10863,#10864,#10865));
#2126=EDGE_LOOP('',(#10866));
#2127=EDGE_LOOP('',(#10867));
#2128=EDGE_LOOP('',(#10868,#10869,#10870,#10871));
#2129=EDGE_LOOP('',(#10872,#10873,#10874,#10875));
#2130=EDGE_LOOP('',(#10876,#10877,#10878,#10879));
#2131=EDGE_LOOP('',(#10880));
#2132=EDGE_LOOP('',(#10881));
#2133=EDGE_LOOP('',(#10882,#10883,#10884,#10885));
#2134=EDGE_LOOP('',(#10886,#10887,#10888,#10889));
#2135=EDGE_LOOP('',(#10890,#10891,#10892,#10893));
#2136=EDGE_LOOP('',(#10894,#10895,#10896,#10897));
#2137=EDGE_LOOP('',(#10898,#10899,#10900,#10901));
#2138=EDGE_LOOP('',(#10902,#10903,#10904,#10905,#10906,#10907,#10908,#10909,
#10910));
#2139=EDGE_LOOP('',(#10911,#10912,#10913,#10914,#10915,#10916,#10917,#10918,
#10919));
#2140=CIRCLE('',#11898,160.);
#2141=CIRCLE('',#11900,170.);
#2142=CIRCLE('',#11901,170.);
#2143=CIRCLE('',#11902,2.5);
#2144=CIRCLE('',#11903,167.5);
#2145=CIRCLE('',#11905,2.5);
#2146=CIRCLE('',#11906,2.5);
#2147=CIRCLE('',#11908,2.5);
#2148=CIRCLE('',#11909,2.5);
#2149=CIRCLE('',#11910,2.5);
#2150=CIRCLE('',#11912,2.5);
#2151=CIRCLE('',#11913,2.5);
#2152=CIRCLE('',#11915,2.5);
#2153=CIRCLE('',#11916,2.5);
#2154=CIRCLE('',#11917,2.5);
#2155=CIRCLE('',#11919,2.5);
#2156=CIRCLE('',#11920,2.5);
#2157=CIRCLE('',#11921,2.49999999999999);
#2158=CIRCLE('',#11923,2.5);
#2159=CIRCLE('',#11924,2.5);
#2160=CIRCLE('',#11925,2.5);
#2161=CIRCLE('',#11927,2.5);
#2162=CIRCLE('',#11928,2.5);
#2163=CIRCLE('',#11929,2.49999999999999);
#2164=CIRCLE('',#11931,194.);
#2165=CIRCLE('',#11932,1.);
#2166=CIRCLE('',#11933,195.);
#2167=CIRCLE('',#11934,195.);
#2168=CIRCLE('',#11936,195.);
#2169=CIRCLE('',#11937,195.);
#2170=CIRCLE('',#11938,1.);
#2171=CIRCLE('',#11939,194.);
#2172=CIRCLE('',#11941,4.49999999999998);
#2173=CIRCLE('',#11942,5.025);
#2174=CIRCLE('',#11944,4.49999999999998);
#2175=CIRCLE('',#11946,4.49999999999998);
#2176=CIRCLE('',#11947,5.025);
#2177=CIRCLE('',#11949,4.49999999999998);
#2178=CIRCLE('',#11951,4.49999999999999);
#2179=CIRCLE('',#11952,5.025);
#2180=CIRCLE('',#11954,4.49999999999997);
#2181=CIRCLE('',#11956,4.49999999999998);
#2182=CIRCLE('',#11957,5.025);
#2183=CIRCLE('',#11959,4.49999999999998);
#2184=CIRCLE('',#11961,4.49999999999998);
#2185=CIRCLE('',#11962,5.025);
#2186=CIRCLE('',#11964,4.49999999999998);
#2187=CIRCLE('',#11966,4.49999999999999);
#2188=CIRCLE('',#11967,5.025);
#2189=CIRCLE('',#11969,4.49999999999998);
#2190=CIRCLE('',#11972,35.5);
#2191=CIRCLE('',#11973,37.5);
#2192=CIRCLE('',#11975,35.5);
#2193=CIRCLE('',#11976,35.5);
#2194=CIRCLE('',#11977,37.5);
#2195=CIRCLE('',#11980,4.5);
#2196=CIRCLE('',#11981,4.5);
#2197=CIRCLE('',#11983,4.5);
#2198=CIRCLE('',#11984,4.5);
#2199=CIRCLE('',#11986,4.5);
#2200=CIRCLE('',#11987,4.5);
#2201=CIRCLE('',#11989,4.5);
#2202=CIRCLE('',#11990,4.5);
#2203=CIRCLE('',#11992,25.);
#2204=CIRCLE('',#11993,25.);
#2205=CIRCLE('',#11995,160.);
#2206=CIRCLE('',#11996,160.);
#2207=CIRCLE('',#11997,160.);
#2208=CIRCLE('',#11999,15.);
#2209=CIRCLE('',#12000,15.);
#2210=CIRCLE('',#12001,15.);
#2211=CIRCLE('',#12002,15.);
#2212=CIRCLE('',#12004,170.);
#2213=CIRCLE('',#12005,170.);
#2214=CIRCLE('',#12006,170.);
#2215=CIRCLE('',#12007,170.);
#2216=CIRCLE('',#12008,170.);
#2217=CIRCLE('',#12009,170.);
#2218=CIRCLE('',#12010,170.);
#2219=CIRCLE('',#12011,170.);
#2220=CIRCLE('',#12012,170.);
#2221=CIRCLE('',#12013,170.);
#2222=CIRCLE('',#12014,170.);
#2223=CIRCLE('',#12015,170.);
#2224=CIRCLE('',#12016,170.);
#2225=CIRCLE('',#12017,170.);
#2226=CIRCLE('',#12018,170.);
#2227=CIRCLE('',#12021,5.);
#2228=CIRCLE('',#12022,5.);
#2229=CIRCLE('',#12023,5.);
#2230=CIRCLE('',#12024,5.);
#2231=CIRCLE('',#12026,5.);
#2232=CIRCLE('',#12027,5.);
#2233=CIRCLE('',#12028,5.);
#2234=CIRCLE('',#12029,5.);
#2235=CIRCLE('',#12032,175.);
#2236=CIRCLE('',#12033,175.);
#2237=CIRCLE('',#12035,210.);
#2238=CIRCLE('',#12036,185.);
#2239=CIRCLE('',#12037,250.);
#2240=CIRCLE('',#12038,135.);
#2241=CIRCLE('',#12040,285.);
#2242=CIRCLE('',#12041,149.388176775342);
#2243=CIRCLE('',#12042,149.388176775134);
#2244=CIRCLE('',#12043,285.);
#2245=CIRCLE('',#12045,250.);
#2246=CIRCLE('',#12046,185.);
#2247=CIRCLE('',#12047,210.);
#2248=CIRCLE('',#12048,135.);
#2249=CIRCLE('',#12059,135.);
#2250=CIRCLE('',#12060,135.);
#2251=CIRCLE('',#12062,137.537590041004);
#2252=CIRCLE('',#12064,137.53759018693);
#2253=CIRCLE('',#12067,80.8416395220943);
#2254=CIRCLE('',#12068,100.);
#2255=CIRCLE('',#12070,100.);
#2256=CIRCLE('',#12071,100.);
#2257=CIRCLE('',#12072,103.415458265314);
#2258=CIRCLE('',#12073,103.415458265742);
#2259=CIRCLE('',#12075,100.);
#2260=CIRCLE('',#12076,80.8416395221478);
#2261=CIRCLE('',#12078,35.);
#2262=CIRCLE('',#12079,35.);
#2263=CIRCLE('',#12080,35.);
#2264=CIRCLE('',#12082,35.);
#2265=CIRCLE('',#12085,35.);
#2266=CIRCLE('',#12086,35.);
#2267=CIRCLE('',#12087,35.);
#2268=CIRCLE('',#12089,35.);
#2269=CIRCLE('',#12092,35.);
#2270=CIRCLE('',#12094,35.);
#2271=CIRCLE('',#12095,35.);
#2272=CIRCLE('',#12098,35.);
#2273=CIRCLE('',#12100,35.);
#2274=CIRCLE('',#12101,35.);
#2275=CIRCLE('',#12103,15.);
#2276=CIRCLE('',#12105,15.);
#2277=CIRCLE('',#12106,15.);
#2278=CIRCLE('',#12108,15.);
#2279=CIRCLE('',#12110,160.);
#2280=CIRCLE('',#12112,185.);
#2281=CIRCLE('',#12113,185.);
#2282=CIRCLE('',#12115,210.);
#2283=CIRCLE('',#12116,135.);
#2284=CIRCLE('',#12117,250.);
#2285=CIRCLE('',#12118,185.);
#2286=CIRCLE('',#12120,275.);
#2287=CIRCLE('',#12121,140.432116498651);
#2288=CIRCLE('',#12122,140.432116498845);
#2289=CIRCLE('',#12123,275.);
#2290=CIRCLE('',#12125,250.);
#2291=CIRCLE('',#12126,135.);
#2292=CIRCLE('',#12127,210.);
#2293=CIRCLE('',#12128,185.);
#2294=CIRCLE('',#12130,135.);
#2295=CIRCLE('',#12131,135.);
#2296=CIRCLE('',#12133,137.537590042586);
#2297=CIRCLE('',#12135,137.537590188513);
#2298=CIRCLE('',#12138,110.);
#2299=CIRCLE('',#12139,91.7232983475876);
#2300=CIRCLE('',#12141,113.104956182355);
#2301=CIRCLE('',#12142,113.104956182419);
#2302=CIRCLE('',#12143,110.);
#2303=CIRCLE('',#12144,110.);
#2304=CIRCLE('',#12146,91.7232983475977);
#2305=CIRCLE('',#12147,110.);
#2306=CIRCLE('',#12149,25.);
#2307=CIRCLE('',#12150,25.);
#2308=CIRCLE('',#12151,25.);
#2309=CIRCLE('',#12153,25.);
#2310=CIRCLE('',#12156,25.);
#2311=CIRCLE('',#12157,25.);
#2312=CIRCLE('',#12158,25.);
#2313=CIRCLE('',#12160,25.);
#2314=CIRCLE('',#12163,25.);
#2315=CIRCLE('',#12165,25.);
#2316=CIRCLE('',#12166,25.);
#2317=CIRCLE('',#12169,25.);
#2318=CIRCLE('',#12171,25.);
#2319=CIRCLE('',#12172,25.);
#2320=CIRCLE('',#12174,25.);
#2321=CIRCLE('',#12176,25.);
#2322=CIRCLE('',#12177,25.);
#2323=CIRCLE('',#12179,25.);
#2324=CIRCLE('',#12183,172.5);
#2325=CIRCLE('',#12185,172.5);
#2326=CIRCLE('',#12188,172.5);
#2327=CIRCLE('',#12190,172.5);
#2328=CIRCLE('',#12193,172.5);
#2329=CIRCLE('',#12195,172.5);
#2330=CIRCLE('',#12198,172.5);
#2331=CIRCLE('',#12200,172.5);
#2332=CIRCLE('',#12203,172.5);
#2333=CIRCLE('',#12205,172.5);
#2334=CIRCLE('',#12208,172.5);
#2335=CIRCLE('',#12210,172.5);
#2336=CIRCLE('',#12218,2.5);
#2337=CIRCLE('',#12220,2.5);
#2338=CIRCLE('',#12222,2.49999999999999);
#2339=CIRCLE('',#12224,2.5);
#2340=CIRCLE('',#12225,2.5);
#2341=CIRCLE('',#12226,2.5);
#2342=CIRCLE('',#12228,2.5);
#2343=CIRCLE('',#12229,2.5);
#2344=CIRCLE('',#12230,2.5);
#2345=CIRCLE('',#12232,2.5);
#2346=CIRCLE('',#12233,2.5);
#2347=CIRCLE('',#12235,2.5);
#2348=CIRCLE('',#12238,2.5);
#2349=CIRCLE('',#12240,2.49999999999999);
#2350=CIRCLE('',#12242,2.5);
#2351=CIRCLE('',#12244,2.5);
#2352=CIRCLE('',#12246,2.49999999999999);
#2353=CIRCLE('',#12248,2.5);
#2354=CIRCLE('',#12250,2.5);
#2355=CIRCLE('',#12252,2.5);
#2356=CIRCLE('',#12253,2.5);
#2357=CIRCLE('',#12255,2.5);
#2358=CIRCLE('',#12257,2.5);
#2359=CIRCLE('',#12258,2.5);
#2360=CIRCLE('',#12260,2.5);
#2361=CIRCLE('',#12262,2.5);
#2362=CIRCLE('',#12263,2.5);
#2363=CIRCLE('',#12265,2.5);
#2364=CIRCLE('',#12268,2.5);
#2365=CIRCLE('',#12270,2.5);
#2366=CIRCLE('',#12272,2.5);
#2367=CIRCLE('',#12275,2.5);
#2368=CIRCLE('',#12277,2.5);
#2369=CIRCLE('',#12278,2.5);
#2370=CIRCLE('',#12280,2.5);
#2371=CIRCLE('',#12282,2.5);
#2372=CIRCLE('',#12285,2.5);
#2373=CIRCLE('',#12287,2.49999999999999);
#2374=CIRCLE('',#12289,2.5);
#2375=CIRCLE('',#12291,2.5);
#2376=CIRCLE('',#12293,2.5);
#2377=CIRCLE('',#12295,2.5);
#2378=CIRCLE('',#12296,2.5);
#2379=CIRCLE('',#12298,2.5);
#2380=CIRCLE('',#12301,2.5);
#2381=CIRCLE('',#12304,2.49999999999999);
#2382=CIRCLE('',#12305,2.5);
#2383=CIRCLE('',#12307,2.5);
#2384=CIRCLE('',#12308,2.5);
#2385=CIRCLE('',#12309,2.5);
#2386=CIRCLE('',#12314,2.5);
#2387=CIRCLE('',#12315,2.5);
#2388=CIRCLE('',#12318,2.5);
#2389=CIRCLE('',#12319,2.5);
#2390=CIRCLE('',#12320,2.5);
#2391=CIRCLE('',#12322,2.5);
#2392=CIRCLE('',#12323,2.5);
#2393=CIRCLE('',#12325,2.5);
#2394=CIRCLE('',#12327,2.5);
#2395=CIRCLE('',#12329,2.5);
#2396=CIRCLE('',#12331,2.5);
#2397=CIRCLE('',#12332,2.5);
#2398=CIRCLE('',#12334,2.5);
#2399=CIRCLE('',#12336,2.5);
#2400=CIRCLE('',#12338,2.5);
#2401=CIRCLE('',#12339,2.5);
#2402=CIRCLE('',#12341,2.5);
#2403=CIRCLE('',#12344,2.5);
#2404=CIRCLE('',#12346,2.5);
#2405=CIRCLE('',#12348,2.49999999999999);
#2406=CIRCLE('',#12351,2.5);
#2407=CIRCLE('',#12352,2.5);
#2408=CIRCLE('',#12354,2.49999999999999);
#2409=CIRCLE('',#12356,2.5);
#2410=CIRCLE('',#12357,2.5);
#2411=CIRCLE('',#12358,2.5);
#2412=CIRCLE('',#12360,2.5);
#2413=CIRCLE('',#12362,2.5);
#2414=CIRCLE('',#12365,2.5);
#2415=CIRCLE('',#12367,2.5);
#2416=CIRCLE('',#12368,2.5);
#2417=CIRCLE('',#12370,2.5);
#2418=CIRCLE('',#12371,2.5);
#2419=CIRCLE('',#12373,2.5);
#2420=CIRCLE('',#12375,2.5);
#2421=CIRCLE('',#12377,2.5);
#2422=CIRCLE('',#12380,2.5);
#2423=CIRCLE('',#12381,2.5);
#2424=CIRCLE('',#12383,2.5);
#2425=CIRCLE('',#12385,2.5);
#2426=CIRCLE('',#12387,2.5);
#2427=CIRCLE('',#12389,2.5);
#2428=CIRCLE('',#12391,2.5);
#2429=CIRCLE('',#12392,2.5);
#2430=CIRCLE('',#12393,2.5);
#2431=CIRCLE('',#12395,2.5);
#2432=CIRCLE('',#12397,2.5);
#2433=CIRCLE('',#12398,2.5);
#2434=CIRCLE('',#12400,2.49999999999999);
#2435=CIRCLE('',#12402,2.49999999999999);
#2436=CIRCLE('',#12404,2.5);
#2437=CIRCLE('',#12406,2.5);
#2438=CIRCLE('',#12409,2.49999999999999);
#2439=CIRCLE('',#12412,2.5);
#2440=CIRCLE('',#12413,2.5);
#2441=CIRCLE('',#12414,2.5);
#2442=CIRCLE('',#12416,2.5);
#2443=CIRCLE('',#12419,2.5);
#2444=CIRCLE('',#12421,2.5);
#2445=CIRCLE('',#12422,2.5);
#2446=CIRCLE('',#12426,37.0000000000001);
#2447=CIRCLE('',#12427,35.);
#2448=CIRCLE('',#12428,35.);
#2449=CIRCLE('',#12430,30.);
#2450=CIRCLE('',#12431,30.);
#2451=CIRCLE('',#12432,29.0000000000001);
#2452=CIRCLE('',#12434,35.);
#2453=CIRCLE('',#12435,35.);
#2454=CIRCLE('',#12436,34.0000000000001);
#2455=CIRCLE('',#12438,9.5);
#2456=CIRCLE('',#12439,9.5);
#2457=CIRCLE('',#12441,120.);
#2458=CIRCLE('',#12442,120.);
#2459=CIRCLE('',#12443,120.);
#2460=CIRCLE('',#12444,120.);
#2461=CIRCLE('',#12445,120.);
#2462=CIRCLE('',#12446,120.);
#2463=CIRCLE('',#12447,120.);
#2464=CIRCLE('',#12448,120.);
#2465=CIRCLE('',#12449,120.);
#2466=CIRCLE('',#12450,120.);
#2467=CIRCLE('',#12451,120.);
#2468=CIRCLE('',#12452,120.);
#2469=CIRCLE('',#12453,120.);
#2470=CIRCLE('',#12454,120.);
#2471=CIRCLE('',#12455,120.);
#2472=CIRCLE('',#12456,120.);
#2473=CIRCLE('',#12457,120.);
#2474=CIRCLE('',#12458,120.);
#2475=CIRCLE('',#12459,120.);
#2476=CIRCLE('',#12460,120.);
#2477=CIRCLE('',#12461,120.);
#2478=CIRCLE('',#12462,120.);
#2479=CIRCLE('',#12464,160.);
#2480=CIRCLE('',#12465,160.);
#2481=CIRCLE('',#12466,160.);
#2482=CIRCLE('',#12467,160.);
#2483=CIRCLE('',#12468,160.);
#2484=CIRCLE('',#12469,160.);
#2485=CIRCLE('',#12470,160.);
#2486=CIRCLE('',#12471,160.);
#2487=CIRCLE('',#12472,160.);
#2488=CIRCLE('',#12473,160.);
#2489=CIRCLE('',#12474,160.);
#2490=CIRCLE('',#12475,160.);
#2491=CIRCLE('',#12476,160.);
#2492=CIRCLE('',#12477,160.);
#2493=CIRCLE('',#12478,160.);
#2494=CIRCLE('',#12479,160.);
#2495=CIRCLE('',#12480,160.);
#2496=CIRCLE('',#12481,160.);
#2497=CIRCLE('',#12482,160.);
#2498=CIRCLE('',#12483,160.);
#2499=CIRCLE('',#12484,160.);
#2500=CIRCLE('',#12485,160.);
#2501=CIRCLE('',#12486,160.);
#2502=CIRCLE('',#12487,160.);
#2503=CIRCLE('',#12490,30.);
#2504=CIRCLE('',#12502,156.);
#2505=CIRCLE('',#12503,156.);
#2506=CIRCLE('',#12504,156.);
#2507=CIRCLE('',#12505,156.);
#2508=CIRCLE('',#12506,156.);
#2509=CIRCLE('',#12507,156.);
#2510=CIRCLE('',#12508,156.);
#2511=CIRCLE('',#12509,156.);
#2512=CIRCLE('',#12510,156.);
#2513=CIRCLE('',#12511,156.);
#2514=CIRCLE('',#12517,10.);
#2515=CIRCLE('',#12519,156.);
#2516=CIRCLE('',#12522,10.);
#2517=CIRCLE('',#12526,10.);
#2518=CIRCLE('',#12528,156.);
#2519=CIRCLE('',#12531,10.);
#2520=CIRCLE('',#12534,10.);
#2521=CIRCLE('',#12536,156.);
#2522=CIRCLE('',#12539,10.);
#2523=CIRCLE('',#12542,10.);
#2524=CIRCLE('',#12544,156.);
#2525=CIRCLE('',#12547,10.);
#2526=CIRCLE('',#12550,10.);
#2527=CIRCLE('',#12552,156.);
#2528=CIRCLE('',#12555,10.);
#2529=CIRCLE('',#12558,10.);
#2530=CIRCLE('',#12560,156.);
#2531=CIRCLE('',#12563,10.);
#2532=CIRCLE('',#12566,10.);
#2533=CIRCLE('',#12568,156.);
#2534=CIRCLE('',#12571,10.);
#2535=CIRCLE('',#12574,10.);
#2536=CIRCLE('',#12576,156.);
#2537=CIRCLE('',#12579,10.);
#2538=CIRCLE('',#12582,10.);
#2539=CIRCLE('',#12584,156.);
#2540=CIRCLE('',#12587,10.);
#2541=CIRCLE('',#12590,10.);
#2542=CIRCLE('',#12592,156.);
#2543=CIRCLE('',#12595,10.);
#2544=CIRCLE('',#12621,194.);
#2545=CIRCLE('',#12622,1.);
#2546=CIRCLE('',#12623,195.);
#2547=CIRCLE('',#12624,195.);
#2548=CIRCLE('',#12626,195.);
#2549=CIRCLE('',#12627,195.);
#2550=CIRCLE('',#12628,1.);
#2551=CIRCLE('',#12629,194.);
#2552=CIRCLE('',#12631,5.50000000000001);
#2553=CIRCLE('',#12632,6.00000000000001);
#2554=CIRCLE('',#12634,5.50000000000001);
#2555=CIRCLE('',#12636,5.50000000000001);
#2556=CIRCLE('',#12637,6.00000000000001);
#2557=CIRCLE('',#12639,5.50000000000001);
#2558=CIRCLE('',#12641,5.5);
#2559=CIRCLE('',#12642,6.);
#2560=CIRCLE('',#12644,5.49999999999999);
#2561=CIRCLE('',#12646,5.50000000000001);
#2562=CIRCLE('',#12647,6.00000000000001);
#2563=CIRCLE('',#12649,5.50000000000001);
#2564=CIRCLE('',#12651,5.50000000000001);
#2565=CIRCLE('',#12652,6.00000000000001);
#2566=CIRCLE('',#12654,5.49999999999998);
#2567=CIRCLE('',#12656,5.5);
#2568=CIRCLE('',#12657,6.);
#2569=CIRCLE('',#12659,5.49999999999999);
#2570=CIRCLE('',#12661,145.);
#2571=CIRCLE('',#12662,145.);
#2572=CIRCLE('',#12670,2.54);
#2573=CIRCLE('',#12671,2.54);
#2574=CIRCLE('',#12674,6.85800000000002);
#2575=CIRCLE('',#12675,6.85800000000002);
#2576=CIRCLE('',#12678,6.85800000000002);
#2577=CIRCLE('',#12679,6.85800000000001);
#2578=CIRCLE('',#12682,2.54);
#2579=CIRCLE('',#12683,2.54);
#2580=CIRCLE('',#12690,2.53999999999999);
#2581=CIRCLE('',#12691,6.85800000000003);
#2582=CIRCLE('',#12692,6.85800000000003);
#2583=CIRCLE('',#12693,2.53999999999999);
#2584=CIRCLE('',#12736,2.54);
#2585=CIRCLE('',#12740,6.858);
#2586=CIRCLE('',#12744,6.85800000000002);
#2587=CIRCLE('',#12748,2.53999999999999);
#2588=CIRCLE('',#12758,2.53999999999999);
#2589=CIRCLE('',#12759,2.53999999999999);
#2590=CIRCLE('',#12762,6.85799999999992);
#2591=CIRCLE('',#12763,6.85799999999992);
#2592=CIRCLE('',#12766,6.85799999999992);
#2593=CIRCLE('',#12767,6.85799999999992);
#2594=CIRCLE('',#12770,2.53999999999999);
#2595=CIRCLE('',#12771,2.53999999999999);
#2596=CIRCLE('',#12778,2.53999999999999);
#2597=CIRCLE('',#12779,6.85800000000003);
#2598=CIRCLE('',#12780,6.85800000000003);
#2599=CIRCLE('',#12781,2.53999999999999);
#2600=CIRCLE('',#12803,2.54);
#2601=CIRCLE('',#12807,6.85800000000003);
#2602=CIRCLE('',#12811,6.85800000000003);
#2603=CIRCLE('',#12815,2.53999999999999);
#2604=CIRCLE('',#12844,2.53999999999999);
#2605=CIRCLE('',#12845,6.85800000000003);
#2606=CIRCLE('',#12846,6.858);
#2607=CIRCLE('',#12847,2.53999999999999);
#2608=CIRCLE('',#12866,2.53999999999999);
#2609=CIRCLE('',#12867,6.858);
#2610=CIRCLE('',#12868,6.85800000000003);
#2611=CIRCLE('',#12869,2.53999999999999);
#2612=CIRCLE('',#12890,3.16991999999999);
#2613=CIRCLE('',#12891,3.16991999999999);
#2614=CIRCLE('',#12894,4.7625);
#2615=CIRCLE('',#12895,4.7625);
#2616=CIRCLE('',#12898,3.16991999999999);
#2617=CIRCLE('',#12899,3.16991999999999);
#2618=CIRCLE('',#12907,3.16991999999999);
#2619=CIRCLE('',#12908,3.16991999999999);
#2620=CIRCLE('',#12911,4.7625);
#2621=CIRCLE('',#12912,4.7625);
#2622=CIRCLE('',#12915,3.16991999999999);
#2623=CIRCLE('',#12916,3.16991999999999);
#2624=CIRCLE('',#12924,3.16991999999999);
#2625=CIRCLE('',#12925,3.16991999999999);
#2626=CIRCLE('',#12928,4.7625);
#2627=CIRCLE('',#12929,4.7625);
#2628=CIRCLE('',#12932,3.16991999999999);
#2629=CIRCLE('',#12933,3.16991999999999);
#2630=CIRCLE('',#12941,3.16991999999999);
#2631=CIRCLE('',#12942,3.16991999999999);
#2632=CIRCLE('',#12945,4.7625);
#2633=CIRCLE('',#12946,4.7625);
#2634=CIRCLE('',#12949,3.16991999999999);
#2635=CIRCLE('',#12950,3.16991999999999);
#2636=CIRCLE('',#12956,3.16991999999999);
#2637=CIRCLE('',#12957,4.7625);
#2638=CIRCLE('',#12958,3.16991999999998);
#2639=CIRCLE('',#12990,3.16991999999996);
#2640=CIRCLE('',#12991,4.7625);
#2641=CIRCLE('',#12992,3.16991999999999);
#2642=CIRCLE('',#13007,3.16991999999996);
#2643=CIRCLE('',#13008,4.7625);
#2644=CIRCLE('',#13009,3.16991999999999);
#2645=CIRCLE('',#13041,3.16991999999999);
#2646=CIRCLE('',#13042,4.7625);
#2647=CIRCLE('',#13043,3.16991999999996);
#2648=CIRCLE('',#13058,4.50000000000006);
#2649=CIRCLE('',#13059,4.49999999999995);
#2650=CIRCLE('',#13061,4.49999999999995);
#2651=CIRCLE('',#13062,4.50000000000006);
#2652=CIRCLE('',#13064,4.49999999999995);
#2653=CIRCLE('',#13065,4.49999999999995);
#2654=CIRCLE('',#13067,4.49999999999995);
#2655=CIRCLE('',#13068,4.49999999999995);
#2656=CIRCLE('',#13074,4.49999999999995);
#2657=CIRCLE('',#13075,4.50000000000006);
#2658=CIRCLE('',#13076,4.49999999999995);
#2659=CIRCLE('',#13077,4.49999999999995);
#2660=CIRCLE('',#13079,4.50000000000006);
#2661=CIRCLE('',#13080,4.49999999999995);
#2662=CIRCLE('',#13081,4.49999999999995);
#2663=CIRCLE('',#13082,4.49999999999995);
#2664=CIRCLE('',#13100,8.74999999999998);
#2665=CIRCLE('',#13101,8.74999999999998);
#2666=CIRCLE('',#13103,8.74999999999998);
#2667=CIRCLE('',#13104,8.74999999999998);
#2668=CIRCLE('',#13128,4.5);
#2669=CIRCLE('',#13129,4.5);
#2670=CIRCLE('',#13131,4.5);
#2671=CIRCLE('',#13132,4.5);
#2672=CIRCLE('',#13136,3.16991999999999);
#2673=CIRCLE('',#13137,3.16991999999999);
#2674=CIRCLE('',#13140,4.7625);
#2675=CIRCLE('',#13141,4.7625);
#2676=CIRCLE('',#13144,3.16991999999999);
#2677=CIRCLE('',#13145,3.16991999999999);
#2678=CIRCLE('',#13151,4.5);
#2679=CIRCLE('',#13152,4.5);
#2680=CIRCLE('',#13154,4.5);
#2681=CIRCLE('',#13155,4.5);
#2682=CIRCLE('',#13159,3.16991999999999);
#2683=CIRCLE('',#13160,3.16991999999999);
#2684=CIRCLE('',#13163,4.7625);
#2685=CIRCLE('',#13164,4.7625);
#2686=CIRCLE('',#13167,3.16991999999999);
#2687=CIRCLE('',#13168,3.16991999999999);
#2688=B_SPLINE_CURVE_WITH_KNOTS('',3,(#16760,#16761,#16762,#16763,#16764,
#16765,#16766,#16767,#16768,#16769,#16770,#16771,#16772,#16773,#16774,#16775,
#16776,#16777,#16778,#16779,#16780,#16781,#16782,#16783,#16784,#16785,#16786,
#16787,#16788,#16789,#16790,#16791,#16792,#16793,#16794,#16795,#16796,#16797,
#16798,#16799,#16800,#16801,#16802,#16803,#16804,#16805),.UNSPECIFIED.,
 .F.,.F.,(4,2,2,2,2,2,2,2,2,2,2,2,2,2,2,2,2,2,2,2,1,1,2,4),(6.93889390390723E-18,
0.012510488710389,0.025020977420778,0.037531466131167,0.0437867104863615,
0.050041954841556,0.0625524435519449,0.0750629322623339,0.0875734209727229,
0.0907010431503202,0.0938286653279175,0.100083909683112,0.12510488710389,
0.137615375814279,0.143870620169474,0.146998242347071,0.150125864524668,
0.175146841945446,0.187657330655835,0.19391257501103,0.197040197188627,
0.198604008277426,0.199385913821825,0.200167819366224),.UNSPECIFIED.);
#2689=B_SPLINE_CURVE_WITH_KNOTS('',3,(#17002,#17003,#17004,#17005,#17006,
#17007,#17008,#17009,#17010,#17011,#17012,#17013,#17014,#17015,#17016,#17017,
#17018,#17019,#17020,#17021,#17022,#17023,#17024,#17025,#17026,#17027,#17028,
#17029,#17030,#17031,#17032,#17033,#17034,#17035,#17036,#17037,#17038,#17039,
#17040,#17041,#17042,#17043,#17044,#17045,#17046,#17047,#17048,#17049,#17050,
#17051,#17052,#17053,#17054,#17055,#17056,#17057,#17058,#17059,#17060,#17061,
#17062,#17063,#17064,#17065,#17066,#17067,#17068,#17069,#17070,#17071,#17072,
#17073,#17074,#17075,#17076,#17077,#17078,#17079,#17080,#17081,#17082,#17083,
#17084,#17085,#17086,#17087,#17088,#17089,#17090,#17091,#17092,#17093,#17094,
#17095,#17096,#17097,#17098,#17099,#17100,#17101,#17102,#17103,#17104,#17105,
#17106,#17107,#17108,#17109,#17110,#17111,#17112,#17113,#17114,#17115,#17116,
#17117,#17118,#17119,#17120,#17121,#17122,#17123,#17124,#17125,#17126,#17127,
#17128,#17129,#17130,#17131,#17132,#17133,#17134,#17135,#17136,#17137,#17138,
#17139,#17140,#17141,#17142,#17143,#17144,#17145,#17146,#17147,#17148,#17149,
#17150,#17151,#17152),.UNSPECIFIED.,.F.,.F.,(4,3,3,3,3,3,3,3,3,3,3,3,3,
3,3,3,3,3,3,3,3,3,3,3,3,3,3,3,3,3,3,3,3,3,3,3,3,3,3,3,3,3,3,3,3,3,3,3,3,
3,4),(0.,0.00264830166754508,0.00338554276768276,0.00615213912871378,0.00675320003132574,
0.00887596942637685,0.0101043537731214,0.0117726415842567,0.0123042782574276,
0.0134347552290183,0.0164143891950787,0.0167346645119878,0.0184564173861414,
0.0200000359794826,0.0215324869504982,0.023233303670992,0.0245199558087172,
0.0246085565148551,0.0248386738910035,0.026435957163951,0.0283935581384038,
0.0296065751333656,0.0307606956435689,0.0327487536070114,0.0351855316944119,
0.0369128347722827,0.0389566060906663,0.0399889043366396,0.0414988150028508,
0.04202602783082,0.0430649739009964,0.0450774572275154,0.0478748168684247,
0.0492171130297102,0.0511362641149651,0.0543446847239159,0.0571422583429271,
0.0606065066150408,0.0615213912871377,0.0631013195616685,0.0645974608514946,
0.0660648494872431,0.0676735304158514,0.0690227825836785,0.0738256695445652,
0.0749288753150223,0.0805294115585075,0.0861299478019928,0.086703763200743,
0.0938021647097608,0.0984342260594203),.UNSPECIFIED.);
#2690=B_SPLINE_CURVE_WITH_KNOTS('',3,(#17154,#17155,#17156,#17157,#17158,
#17159,#17160,#17161,#17162,#17163,#17164,#17165,#17166,#17167,#17168,#17169,
#17170,#17171,#17172,#17173,#17174,#17175,#17176,#17177,#17178,#17179,#17180,
#17181,#17182,#17183,#17184,#17185,#17186,#17187,#17188,#17189,#17190,#17191,
#17192,#17193,#17194,#17195,#17196,#17197,#17198,#17199,#17200,#17201,#17202,
#17203,#17204,#17205,#17206,#17207,#17208,#17209,#17210,#17211,#17212,#17213,
#17214,#17215,#17216,#17217,#17218,#17219,#17220,#17221,#17222,#17223,#17224,
#17225,#17226,#17227,#17228,#17229,#17230,#17231,#17232,#17233,#17234,#17235,
#17236,#17237,#17238,#17239,#17240,#17241,#17242,#17243,#17244,#17245,#17246,
#17247,#17248,#17249,#17250,#17251,#17252,#17253,#17254,#17255,#17256,#17257,
#17258,#17259,#17260,#17261,#17262,#17263,#17264,#17265,#17266,#17267,#17268,
#17269,#17270,#17271,#17272,#17273,#17274,#17275,#17276,#17277,#17278,#17279,
#17280,#17281,#17282,#17283,#17284,#17285,#17286,#17287,#17288,#17289,#17290,
#17291,#17292,#17293,#17294,#17295,#17296,#17297,#17298,#17299,#17300,#17301),
 .UNSPECIFIED.,.F.,.F.,(4,3,3,3,3,3,3,3,3,3,3,3,3,3,3,3,3,3,3,3,3,3,3,3,
3,3,3,3,3,3,3,3,3,3,3,3,3,3,3,3,3,3,3,3,3,3,3,3,3,4),(0.,0.00699935009771002,
0.0115878817442571,0.0121530384978837,0.0176872713323866,0.0232215041668896,
0.0243060769957673,0.0290574768221091,0.0303825962447091,0.0319809849768297,
0.03342085586918,0.0349085984995057,0.0364591154936509,0.0398781022204002,
0.0407914186220395,0.0439575936087226,0.0467217721965195,0.0486121539915344,
0.0513731746692753,0.0527047635302581,0.0546886732404762,0.0557181757572648,
0.0571822792019564,0.0577269328649471,0.058749934730288,0.060765192489418,
0.0631518430351688,0.0648815331197537,0.0668417117383597,0.0679851377317531,
0.0698799713628306,0.0711170083048033,0.0726138269890378,0.0729182309873014,
0.0742789219025961,0.0769869909005962,0.0774720533494774,0.0789947502362431,
0.0806965684066139,0.0820330098607139,0.0839556611802726,0.0850712694851847,
0.0855980872713523,0.0872458532651735,0.0902536243928731,0.0905546388244349,
0.0911477887341263,0.0938804422276097,0.096465786429821,0.097224307983068),
 .UNSPECIFIED.);
#2691=B_SPLINE_CURVE_WITH_KNOTS('',3,(#17305,#17306,#17307,#17308,#17309,
#17310,#17311,#17312,#17313,#17314,#17315,#17316,#17317,#17318,#17319,#17320,
#17321,#17322,#17323,#17324,#17325,#17326,#17327,#17328,#17329,#17330,#17331,
#17332,#17333,#17334,#17335,#17336,#17337,#17338,#17339,#17340,#17341,#17342,
#17343,#17344,#17345,#17346,#17347,#17348,#17349,#17350),.UNSPECIFIED.,
 .F.,.F.,(4,2,1,1,2,2,2,2,2,2,2,2,2,2,2,2,2,2,2,2,2,2,2,4),(-0.000149655236900613,
0.000631565722958083,0.00141278668281678,0.00297522860253417,0.00610011244196896,
0.0123498801208385,0.0248494154785777,0.0498484861940559,0.0529733700334907,
0.0560982538729255,0.0623480215517949,0.074847556909534,0.0998466276250119,
0.106096395303881,0.109221279143316,0.112346162982751,0.12484569834049,
0.137345233698229,0.149844769055968,0.156094536734838,0.162344304413707,
0.174843839771446,0.187343375129185,0.199842910486925),.UNSPECIFIED.);
#2692=B_SPLINE_CURVE_WITH_KNOTS('',3,(#17377,#17378,#17379,#17380,#17381,
#17382,#17383,#17384,#17385,#17386,#17387,#17388,#17389,#17390,#17391,#17392,
#17393,#17394,#17395,#17396,#17397,#17398,#17399,#17400,#17401,#17402,#17403,
#17404,#17405,#17406,#17407,#17408,#17409,#17410,#17411,#17412,#17413,#17414,
#17415,#17416,#17417,#17418,#17419,#17420,#17421,#17422),.UNSPECIFIED.,
 .F.,.F.,(4,2,1,1,2,2,2,2,2,2,2,2,2,2,2,2,2,2,2,2,2,2,2,4),(-0.000143873254053562,
0.00068268999816279,0.00150925325037914,0.00316237975481185,0.00646863276367728,
0.0130811387814081,0.0263061508168699,0.0527561748877933,0.0560624278966588,
0.0593686809055243,0.0659811869232552,0.0792061989587171,0.105656223029641,
0.112268729047372,0.115574982056237,0.118881235065103,0.132106247100564,
0.145331259136026,0.158556271171488,0.165168777189219,0.17178128320695,
0.185006295242412,0.198231307277874,0.211456319313335),.UNSPECIFIED.);
#2693=B_SPLINE_CURVE_WITH_KNOTS('',3,(#17425,#17426,#17427,#17428,#17429,
#17430,#17431,#17432,#17433,#17434,#17435,#17436,#17437,#17438,#17439,#17440,
#17441,#17442,#17443,#17444,#17445,#17446,#17447,#17448,#17449,#17450,#17451,
#17452,#17453,#17454,#17455,#17456,#17457,#17458,#17459,#17460,#17461,#17462,
#17463,#17464,#17465,#17466,#17467,#17468,#17469,#17470,#17471,#17472,#17473,
#17474,#17475,#17476,#17477,#17478,#17479,#17480,#17481,#17482,#17483,#17484,
#17485,#17486,#17487,#17488,#17489,#17490,#17491,#17492,#17493,#17494,#17495,
#17496,#17497,#17498,#17499,#17500,#17501,#17502,#17503,#17504,#17505,#17506,
#17507,#17508,#17509,#17510,#17511,#17512,#17513,#17514,#17515,#17516,#17517,
#17518,#17519,#17520,#17521,#17522,#17523,#17524,#17525,#17526,#17527,#17528,
#17529,#17530,#17531,#17532,#17533,#17534,#17535,#17536,#17537,#17538,#17539,
#17540,#17541,#17542,#17543,#17544,#17545,#17546,#17547,#17548,#17549,#17550,
#17551,#17552,#17553,#17554,#17555,#17556,#17557,#17558,#17559,#17560,#17561,
#17562,#17563,#17564,#17565,#17566,#17567,#17568,#17569,#17570,#17571,#17572),
 .UNSPECIFIED.,.F.,.F.,(4,3,3,3,3,3,3,3,3,3,3,3,3,3,3,3,3,3,3,3,3,3,3,3,
3,3,3,3,3,3,3,3,3,3,3,3,3,3,3,3,3,3,3,3,3,3,3,3,3,4),(0.,0.00881316361102408,
0.012318109623398,0.012654007285576,0.0192322733979474,0.0246628334681499,
0.025308014571152,0.0308463442051709,0.03163501821394,0.0339412090926062,
0.034798520035334,0.0366217278304301,0.0370385678531182,0.037962021856728,
0.0420896412580113,0.0432496109903109,0.0470627457271248,0.0494885274351577,
0.050616029142304,0.0539401501903541,0.0557583986413853,0.056943032785092,
0.0589060145066337,0.060106534606486,0.0619089996968021,0.0620646425562423,
0.06327003642788,0.0660634006959954,0.0684230551784283,0.0695970400706682,
0.0723641943522411,0.0748437627090561,0.0759240437134563,0.0776293975979093,
0.0780803908188895,0.0790875455348503,0.0813357451113595,0.0822510473562443,
0.0846104548920026,0.0868029327330513,0.0879062841801969,0.0885780509990324,
0.0895621613745393,0.0912212332537684,0.0917415528204264,0.0945473329030429,
0.0949050546418204,0.0978841144285108,0.100727891650727,0.101232058284608),
 .UNSPECIFIED.);
#2694=B_SPLINE_CURVE_WITH_KNOTS('',3,(#17574,#17575,#17576,#17577,#17578,
#17579,#17580,#17581,#17582,#17583,#17584,#17585,#17586,#17587,#17588,#17589,
#17590,#17591,#17592,#17593,#17594,#17595,#17596,#17597,#17598,#17599,#17600,
#17601,#17602,#17603,#17604,#17605,#17606,#17607,#17608,#17609,#17610,#17611,
#17612,#17613,#17614,#17615,#17616,#17617,#17618,#17619,#17620,#17621,#17622,
#17623,#17624,#17625,#17626,#17627,#17628,#17629,#17630,#17631,#17632,#17633,
#17634,#17635,#17636,#17637,#17638,#17639,#17640,#17641,#17642,#17643,#17644,
#17645,#17646,#17647,#17648,#17649,#17650,#17651,#17652,#17653,#17654,#17655,
#17656,#17657,#17658,#17659,#17660,#17661,#17662,#17663,#17664,#17665,#17666,
#17667,#17668,#17669,#17670,#17671,#17672,#17673,#17674,#17675,#17676,#17677,
#17678,#17679,#17680,#17681,#17682,#17683,#17684,#17685,#17686,#17687,#17688,
#17689,#17690,#17691,#17692,#17693,#17694,#17695,#17696,#17697,#17698,#17699,
#17700,#17701,#17702,#17703,#17704,#17705,#17706,#17707,#17708,#17709,#17710,
#17711,#17712,#17713,#17714,#17715,#17716,#17717,#17718,#17719,#17720,#17721,
#17722,#17723,#17724,#17725,#17726,#17727,#17728,#17729,#17730,#17731,#17732,
#17733,#17734,#17735,#17736,#17737,#17738,#17739),.UNSPECIFIED.,.F.,.F.,
(4,3,3,3,3,3,3,3,3,3,3,3,3,3,3,3,3,3,3,3,3,3,3,3,3,3,3,3,3,3,3,3,3,3,3,
3,3,3,3,3,3,3,3,3,3,3,3,3,3,3,3,3,3,3,3,4),(2.08166817117217E-17,0.00290669333800962,
0.00338285849467252,0.00638266577622659,0.00675466553082774,0.00957399866433987,
0.0101158798388015,0.0111696651083965,0.0117924346723956,0.0127653315524531,
0.0134658165946075,0.0154513391424759,0.0167960113431925,0.0188942944985078,
0.0191479973286796,0.020104902412734,0.0223393302167929,0.0233947318771642,
0.0248446076333751,0.0250326894729064,0.0255306631049062,0.0266657591960594,
0.0290802964524566,0.0315436764715739,0.0319133288811327,0.0331530367439499,
0.0359945749075088,0.0382959946573593,0.0395777786403494,0.0411983131160884,
0.0414873275454726,0.0427687325086115,0.0446786604335859,0.0459499786559523,
0.0493101507548442,0.0510613262098124,0.0522860562858319,0.056141541692772,
0.0585911480323024,0.0627635580079887,0.0638266577622654,0.0648685301336492,
0.0675785692393606,0.0679976842497239,0.0702093235384919,0.0711211657829561,
0.0757381109941175,0.0765919893147184,0.0773525560315269,0.0826886438907914,
0.0881008269604734,0.0893573208671715,0.0897580784854174,0.095739986643398,
0.0989313195315113,0.102122652419625),.UNSPECIFIED.);
#2695=B_SPLINE_CURVE_WITH_KNOTS('',3,(#17742,#17743,#17744,#17745,#17746,
#17747,#17748,#17749,#17750,#17751,#17752,#17753,#17754,#17755,#17756,#17757,
#17758,#17759,#17760,#17761,#17762,#17763,#17764,#17765,#17766,#17767,#17768,
#17769,#17770,#17771,#17772,#17773,#17774,#17775,#17776,#17777,#17778,#17779,
#17780,#17781,#17782,#17783,#17784,#17785,#17786,#17787),.UNSPECIFIED.,
 .F.,.F.,(4,2,2,2,2,2,2,2,2,2,2,2,2,2,2,2,2,2,2,2,1,1,2,4),(0.,0.0132405753593167,
0.0264811507186334,0.03972172607795,0.0463420137576084,0.0529623014372667,
0.0662028767965833,0.0794434521559,0.0926840275152166,0.0959941713550458,
0.099304315194875,0.105924602874533,0.132405753593167,0.145646328952484,
0.152266616632142,0.155576760471971,0.158886904311801,0.185368055030434,
0.198608630389751,0.205228918069409,0.208539061909239,0.210194133829153,
0.211021669789111,0.211849205749068),.UNSPECIFIED.);
#2696=B_SPLINE_CURVE_WITH_KNOTS('',3,(#17791,#17792,#17793,#17794,#17795,
#17796,#17797,#17798,#17799,#17800,#17801,#17802,#17803,#17804,#17805,#17806,
#17807,#17808,#17809,#17810,#17811,#17812,#17813,#17814,#17815,#17816,#17817,
#17818,#17819,#17820,#17821,#17822,#17823,#17824,#17825,#17826,#17827,#17828,
#17829,#17830,#17831,#17832,#17833,#17834,#17835,#17836,#17837,#17838,#17839,
#17840,#17841,#17842,#17843,#17844,#17845,#17846,#17847,#17848,#17849,#17850,
#17851,#17852,#17853,#17854,#17855,#17856,#17857,#17858,#17859,#17860,#17861,
#17862,#17863,#17864,#17865,#17866,#17867,#17868,#17869,#17870,#17871,#17872,
#17873,#17874,#17875),.UNSPECIFIED.,.F.,.F.,(4,3,3,3,3,3,3,3,3,3,3,3,3,
3,3,3,3,3,3,3,3,3,3,3,3,3,3,3,4),(0.,0.00210238164606691,0.00298624731337001,
0.00299593240969137,0.00448011523757044,0.00449389861453705,0.00556805401174092,
0.00597475171775576,0.00599186481938273,0.00694008292290932,0.0074710492535578,
0.00748983102422842,0.00823006541652398,0.00891808975407265,0.00897029980881955,
0.0089877972290741,0.00949013839786762,0.00972165589821712,0.00973678033149696,
0.0102479898279996,0.0104747574652596,0.0104857634339198,0.0109645659632965,
0.0112298884386646,0.0112347465363427,0.0114330324441498,0.0116282685995547,
0.0118121268564596,0.0119837296387656),.UNSPECIFIED.);
#2697=B_SPLINE_CURVE_WITH_KNOTS('',3,(#17879,#17880,#17881,#17882,#17883,
#17884,#17885,#17886,#17887,#17888,#17889,#17890,#17891,#17892,#17893,#17894,
#17895,#17896,#17897,#17898,#17899,#17900,#17901,#17902,#17903,#17904,#17905,
#17906,#17907,#17908,#17909,#17910,#17911,#17912,#17913,#17914,#17915,#17916,
#17917,#17918,#17919,#17920,#17921,#17922,#17923,#17924,#17925,#17926,#17927,
#17928,#17929,#17930,#17931,#17932,#17933,#17934,#17935,#17936,#17937,#17938,
#17939,#17940,#17941,#17942,#17943,#17944,#17945,#17946,#17947,#17948,#17949,
#17950,#17951,#17952,#17953,#17954,#17955,#17956,#17957),.UNSPECIFIED.,
 .F.,.F.,(4,3,3,3,3,3,3,3,3,3,3,3,3,3,3,3,3,3,3,3,3,3,3,3,3,3,4),(0.,0.000757222794088626,
0.000765731273283226,0.00122273697568558,0.00151444558817725,0.00152974002781745,
0.0019409865546434,0.00227166838226588,0.00229159621626168,0.00278415722201324,
0.00302889117635451,0.00305168138595085,0.00378611397044313,0.00381043827612813,
0.00454333676453176,0.00456831455729546,0.00568821706947207,0.00605778235270903,
0.00608221480188253,0.00735604281924785,0.00757222794088631,0.00759402974301736,
0.00884048373849979,0.00908667352906358,0.0091034204318894,0.0112259507413396,
0.0121155647054181),.UNSPECIFIED.);
#2698=B_SPLINE_CURVE_WITH_KNOTS('',3,(#17960,#17961,#17962,#17963,#17964,
#17965,#17966,#17967,#17968,#17969,#17970,#17971,#17972,#17973,#17974,#17975,
#17976,#17977,#17978,#17979,#17980,#17981,#17982,#17983,#17984,#17985,#17986,
#17987,#17988,#17989,#17990,#17991,#17992,#17993,#17994,#17995,#17996,#17997,
#17998,#17999,#18000,#18001,#18002,#18003,#18004,#18005,#18006,#18007,#18008,
#18009,#18010,#18011,#18012,#18013,#18014,#18015,#18016,#18017,#18018,#18019,
#18020,#18021,#18022,#18023,#18024,#18025,#18026,#18027,#18028,#18029,#18030,
#18031,#18032,#18033,#18034,#18035,#18036,#18037,#18038,#18039,#18040,#18041,
#18042,#18043,#18044),.UNSPECIFIED.,.F.,.F.,(4,3,3,3,3,3,3,3,3,3,3,3,3,
3,3,3,3,3,3,3,3,3,3,3,3,3,3,3,4),(0.,0.00148924028645351,0.00237768466992159,
0.00240031428091277,0.00307153272987116,0.00357468500117901,0.00360047142136915,
0.00432197233413991,0.00477356764211708,0.00480062856182553,0.00528862367612776,
0.00537382713867285,0.00540070713205373,0.00597487440961078,0.00600078570228193,
0.00645684171978798,0.00657682867032061,0.00660086427251013,0.00704835769067905,
0.00717981783844028,0.00720094284273833,0.00766097488130279,0.00778383982492896,
0.00780102141296652,0.00829799353416695,0.00838897096983566,0.00840109998319472,
0.00899484866798043,0.00960125712365108),.UNSPECIFIED.);
#2699=B_SPLINE_CURVE_WITH_KNOTS('',3,(#18048,#18049,#18050,#18051,#18052,
#18053,#18054,#18055,#18056,#18057,#18058,#18059,#18060,#18061,#18062,#18063,
#18064,#18065,#18066,#18067,#18068,#18069,#18070,#18071,#18072,#18073,#18074,
#18075,#18076,#18077,#18078,#18079,#18080,#18081,#18082,#18083,#18084,#18085,
#18086,#18087,#18088,#18089,#18090,#18091,#18092,#18093,#18094,#18095,#18096,
#18097,#18098,#18099,#18100,#18101,#18102,#18103,#18104,#18105,#18106,#18107,
#18108,#18109,#18110,#18111,#18112,#18113,#18114,#18115,#18116,#18117,#18118,
#18119,#18120,#18121,#18122,#18123,#18124,#18125,#18126),.UNSPECIFIED.,
 .F.,.F.,(4,3,3,3,3,3,3,3,3,3,3,3,3,3,3,3,3,3,3,3,3,3,3,3,3,3,4),(0.,0.00162299209129682,
0.00263692856163744,0.00264790906062433,0.00395638686476062,0.0039718635909365,
0.00485040334252278,0.00527680482969886,0.00529581812124867,0.00622095880290044,
0.00659932264757816,0.00661977265156084,0.00736112912107425,0.00792503767209058,
0.00794372718187301,0.00841598728205416,0.00858967996918311,0.00860570444702908,
0.00906736572635407,0.00925571685290464,0.00926768171218515,0.00981205664257965,
0.00992324054391518,0.00992965897734122,0.0102427913968407,0.0105469048764859,
0.0105916362424973),.UNSPECIFIED.);
#2700=B_SPLINE_CURVE_WITH_KNOTS('',3,(#18130,#18131,#18132,#18133,#18134,
#18135,#18136,#18137,#18138,#18139,#18140,#18141,#18142,#18143,#18144,#18145,
#18146,#18147,#18148,#18149,#18150,#18151,#18152,#18153,#18154,#18155,#18156,
#18157,#18158,#18159,#18160,#18161,#18162,#18163,#18164,#18165,#18166,#18167,
#18168,#18169,#18170,#18171,#18172,#18173,#18174,#18175,#18176,#18177,#18178,
#18179,#18180,#18181,#18182,#18183,#18184,#18185,#18186,#18187,#18188,#18189,
#18190,#18191,#18192,#18193,#18194,#18195,#18196,#18197,#18198,#18199,#18200,
#18201,#18202,#18203,#18204,#18205),.UNSPECIFIED.,.F.,.F.,(4,3,3,3,3,3,
3,3,3,3,3,3,3,3,3,3,3,3,3,3,3,3,3,3,3,4),(0.,0.000670198241349187,0.000677695014211876,
0.00121178630208934,0.00134039648269837,0.00135448412697923,0.00180065626354131,
0.00201059472404756,0.00202974735023087,0.00248224413553994,0.00268079296539675,
0.00270360746120654,0.00357365375947468,0.00402118944809509,0.0040477069870127,
0.0048143151556897,0.00536158593079343,0.00538862458081482,0.00657578263990178,
0.00670198241349178,0.00672748973794272,0.00773324143869607,0.00804237889619012,
0.00806372813653269,0.00982128265372075,0.0107231718615868),
 .UNSPECIFIED.);
#2701=B_SPLINE_CURVE_WITH_KNOTS('',3,(#18208,#18209,#18210,#18211,#18212,
#18213,#18214,#18215,#18216,#18217,#18218,#18219,#18220,#18221,#18222,#18223,
#18224,#18225,#18226,#18227,#18228,#18229,#18230,#18231,#18232,#18233,#18234,
#18235,#18236,#18237,#18238,#18239,#18240,#18241,#18242,#18243,#18244,#18245,
#18246,#18247,#18248,#18249,#18250,#18251,#18252,#18253,#18254,#18255,#18256,
#18257,#18258,#18259,#18260,#18261,#18262,#18263,#18264,#18265,#18266,#18267,
#18268,#18269,#18270,#18271,#18272,#18273,#18274,#18275,#18276,#18277,#18278,
#18279,#18280,#18281,#18282,#18283,#18284,#18285,#18286,#18287,#18288,#18289),
 .UNSPECIFIED.,.F.,.F.,(4,3,3,3,3,3,3,3,3,3,3,3,3,3,3,3,3,3,3,3,3,3,3,3,
3,3,3,4),(0.,0.000605114434157146,0.000605179022010971,0.000885247098200934,
0.00117911739500317,0.00121035804402194,0.00121482791364222,0.00181553706603291,
0.00182453317148372,0.00233958065168244,0.00242071608804389,0.00243323369215932,
0.00345385286359851,0.00363107413206585,0.00364741411510169,0.00419813513985867,
0.00423625315407682,0.0042530657539622,0.00484143217608779,0.00485798624729427,
0.00592735701347183,0.00605179022010966,0.00606599525117838,0.00700618113292556,
0.00726214826413153,0.00727234538984921,0.00902506966773751,0.00968286435217533),
 .UNSPECIFIED.);
#2702=B_SPLINE_CURVE_WITH_KNOTS('',3,(#18293,#18294,#18295,#18296,#18297,
#18298,#18299,#18300,#18301,#18302,#18303,#18304,#18305,#18306,#18307,#18308,
#18309,#18310,#18311,#18312,#18313,#18314,#18315,#18316,#18317,#18318,#18319,
#18320,#18321,#18322,#18323,#18324,#18325,#18326,#18327,#18328,#18329,#18330,
#18331,#18332,#18333,#18334,#18335,#18336,#18337,#18338,#18339,#18340,#18341,
#18342,#18343,#18344,#18345,#18346,#18347,#18348,#18349,#18350,#18351,#18352,
#18353,#18354,#18355,#18356,#18357,#18358,#18359,#18360,#18361,#18362,#18363,
#18364,#18365,#18366,#18367,#18368,#18369,#18370,#18371,#18372,#18373,#18374,
#18375,#18376,#18377),.UNSPECIFIED.,.F.,.F.,(4,3,3,3,3,3,3,3,3,3,3,3,3,
3,3,3,3,3,3,3,3,3,3,3,3,3,3,3,4),(0.,0.00210238158617021,0.00298624731337001,
0.00299593240969137,0.00448011523757043,0.00449389861453705,0.00556805401504983,
0.00597475171775576,0.00599186481938273,0.00694008292510282,0.00747104925355784,
0.00748983102422842,0.008230065416524,0.00891808975449004,0.00897029980881959,
0.0089877972290741,0.00949013839878191,0.00972165589821711,0.00973678033149696,
0.0102479898273787,0.0104747574652596,0.0104857634339198,0.0109645659632669,
0.0112298884386646,0.0112347465363427,0.0114330324441506,0.0116282685995556,
0.0118121268564602,0.0119837296387656),.UNSPECIFIED.);
#2703=B_SPLINE_CURVE_WITH_KNOTS('',3,(#18381,#18382,#18383,#18384,#18385,
#18386,#18387,#18388,#18389,#18390,#18391,#18392,#18393,#18394,#18395,#18396,
#18397,#18398,#18399,#18400,#18401,#18402,#18403,#18404,#18405,#18406,#18407,
#18408,#18409,#18410,#18411,#18412,#18413,#18414,#18415,#18416,#18417,#18418,
#18419,#18420,#18421,#18422,#18423,#18424,#18425,#18426,#18427,#18428,#18429,
#18430,#18431,#18432,#18433,#18434,#18435,#18436,#18437,#18438,#18439,#18440,
#18441,#18442,#18443,#18444,#18445,#18446,#18447,#18448,#18449,#18450,#18451,
#18452,#18453,#18454,#18455,#18456,#18457,#18458,#18459),.UNSPECIFIED.,
 .F.,.F.,(4,3,3,3,3,3,3,3,3,3,3,3,3,3,3,3,3,3,3,3,3,3,3,3,3,3,4),(0.,0.000757222794088626,
0.000765731273283215,0.00122273697570158,0.00151444558817725,0.00152974002781745,
0.00194098655463584,0.00227166838226588,0.00229159621626168,0.00278415722201872,
0.00302889117635451,0.00305168138595085,0.00378611397044313,0.00381043827612816,
0.00454333676453176,0.00456831455729547,0.00568821706947819,0.00605778235270903,
0.00608221480188252,0.00735604281927811,0.00757222794088631,0.00759402974301739,
0.00884048373847147,0.00908667352906358,0.00910342043188939,0.0112259507411916,
0.0121155647054181),.UNSPECIFIED.);
#2704=B_SPLINE_CURVE_WITH_KNOTS('',3,(#18464,#18465,#18466,#18467,#18468,
#18469,#18470,#18471,#18472,#18473,#18474,#18475,#18476,#18477,#18478,#18479,
#18480,#18481,#18482,#18483,#18484,#18485,#18486,#18487,#18488,#18489,#18490,
#18491,#18492,#18493,#18494,#18495,#18496,#18497,#18498,#18499,#18500,#18501,
#18502,#18503,#18504,#18505,#18506,#18507,#18508,#18509,#18510,#18511,#18512,
#18513,#18514,#18515,#18516,#18517,#18518,#18519,#18520,#18521,#18522,#18523,
#18524,#18525,#18526,#18527,#18528,#18529,#18530,#18531,#18532,#18533,#18534,
#18535,#18536,#18537,#18538,#18539,#18540,#18541,#18542,#18543,#18544,#18545,
#18546,#18547,#18548),.UNSPECIFIED.,.F.,.F.,(4,3,3,3,3,3,3,3,3,3,3,3,3,
3,3,3,3,3,3,3,3,3,3,3,3,3,3,3,4),(0.,0.00210238158617021,0.00298624731337001,
0.00299593240969137,0.00448011523757043,0.00449389861453705,0.00556805401504983,
0.00597475171775576,0.00599186481938273,0.00694008292510282,0.00747104925355784,
0.00748983102422842,0.008230065416524,0.00891808975449004,0.00897029980881959,
0.0089877972290741,0.00949013839878191,0.00972165589821711,0.00973678033149696,
0.0102479898273787,0.0104747574652596,0.0104857634339198,0.0109645659632669,
0.0112298884386646,0.0112347465363427,0.0114330324441506,0.0116282685995556,
0.0118121268564602,0.0119837296387656),.UNSPECIFIED.);
#2705=B_SPLINE_CURVE_WITH_KNOTS('',3,(#18552,#18553,#18554,#18555,#18556,
#18557,#18558,#18559,#18560,#18561,#18562,#18563,#18564,#18565,#18566,#18567,
#18568,#18569,#18570,#18571,#18572,#18573,#18574,#18575,#18576,#18577,#18578,
#18579,#18580,#18581,#18582,#18583,#18584,#18585,#18586,#18587,#18588,#18589,
#18590,#18591,#18592,#18593,#18594,#18595,#18596,#18597,#18598,#18599,#18600,
#18601,#18602,#18603,#18604,#18605,#18606,#18607,#18608,#18609,#18610,#18611,
#18612,#18613,#18614,#18615,#18616,#18617,#18618,#18619,#18620,#18621,#18622,
#18623,#18624,#18625,#18626,#18627,#18628,#18629,#18630),.UNSPECIFIED.,
 .F.,.F.,(4,3,3,3,3,3,3,3,3,3,3,3,3,3,3,3,3,3,3,3,3,3,3,3,3,3,4),(0.,0.000757222794088626,
0.000765731273283228,0.00122273697432919,0.00151444558817725,0.00152974002781744,
0.00194098655327453,0.00227166838226588,0.00229159621626166,0.00278415722112148,
0.00302889117635451,0.00305168138595084,0.00378611397044313,0.00381043827612816,
0.00454333676453176,0.00456831455729547,0.00568821706029033,0.00605778235270903,
0.00608221480188251,0.00735604281963548,0.00757222794088631,0.00759402974301735,
0.0088404837342444,0.00908667352906358,0.00910342043188939,0.0112259507925462,
0.0121155647054181),.UNSPECIFIED.);
#2706=B_SPLINE_CURVE_WITH_KNOTS('',3,(#18636,#18637,#18638,#18639,#18640,
#18641,#18642,#18643,#18644,#18645,#18646,#18647,#18648,#18649,#18650,#18651,
#18652,#18653,#18654,#18655,#18656,#18657,#18658,#18659,#18660,#18661,#18662,
#18663,#18664,#18665,#18666,#18667,#18668,#18669,#18670,#18671,#18672,#18673,
#18674,#18675,#18676,#18677,#18678,#18679,#18680,#18681,#18682,#18683,#18684,
#18685,#18686,#18687,#18688,#18689,#18690,#18691,#18692,#18693,#18694,#18695,
#18696,#18697,#18698,#18699,#18700,#18701,#18702,#18703,#18704,#18705,#18706,
#18707,#18708,#18709,#18710,#18711,#18712,#18713,#18714,#18715,#18716,#18717,
#18718,#18719,#18720),.UNSPECIFIED.,.F.,.F.,(4,3,3,3,3,3,3,3,3,3,3,3,3,
3,3,3,3,3,3,3,3,3,3,3,3,3,3,3,4),(0.,0.00210238158611208,0.00298624731337002,
0.00299593240969137,0.00448011523757044,0.00449389861453705,0.00556805401505052,
0.00597475171775575,0.00599186481938273,0.00694008292511326,0.00747104925355785,
0.00748983102422842,0.008230065416524,0.00891808975448554,0.00897029980881958,
0.0089877972290741,0.00949013839877169,0.0097216558982171,0.00973678033149696,
0.0102479898273712,0.0104747574652596,0.0104857634339198,0.0109645659632994,
0.0112298884386646,0.0112347465363427,0.0114330324441497,0.0116282685995542,
0.011812126856459,0.0119837296387656),.UNSPECIFIED.);
#2707=B_SPLINE_CURVE_WITH_KNOTS('',3,(#18724,#18725,#18726,#18727,#18728,
#18729,#18730,#18731,#18732,#18733,#18734,#18735,#18736,#18737,#18738,#18739,
#18740,#18741,#18742,#18743,#18744,#18745,#18746,#18747,#18748,#18749,#18750,
#18751,#18752,#18753,#18754,#18755,#18756,#18757,#18758,#18759,#18760,#18761,
#18762,#18763,#18764,#18765,#18766,#18767,#18768,#18769,#18770,#18771,#18772,
#18773,#18774,#18775,#18776,#18777,#18778,#18779,#18780,#18781,#18782,#18783,
#18784,#18785,#18786,#18787,#18788,#18789,#18790,#18791,#18792,#18793,#18794,
#18795,#18796,#18797,#18798,#18799,#18800,#18801,#18802),.UNSPECIFIED.,
 .F.,.F.,(4,3,3,3,3,3,3,3,3,3,3,3,3,3,3,3,3,3,3,3,3,3,3,3,3,3,4),(0.,0.000757222794088626,
0.000765731273283226,0.00122273697568558,0.00151444558817725,0.00152974002781745,
0.0019409865546434,0.00227166838226588,0.00229159621626168,0.00278415722201324,
0.00302889117635451,0.00305168138595085,0.00378611397044313,0.00381043827612813,
0.00454333676453176,0.00456831455729546,0.00568821706947207,0.00605778235270903,
0.00608221480188253,0.00735604281924785,0.00757222794088631,0.00759402974301736,
0.00884048373849979,0.00908667352906358,0.0091034204318894,0.0112259507413396,
0.0121155647054181),.UNSPECIFIED.);
#2708=B_SPLINE_CURVE_WITH_KNOTS('',3,(#18807,#18808,#18809,#18810,#18811,
#18812,#18813,#18814,#18815,#18816,#18817,#18818,#18819,#18820,#18821,#18822,
#18823,#18824,#18825,#18826,#18827,#18828,#18829,#18830,#18831,#18832,#18833,
#18834,#18835,#18836,#18837,#18838,#18839,#18840,#18841,#18842,#18843,#18844,
#18845,#18846,#18847,#18848,#18849,#18850,#18851,#18852,#18853,#18854,#18855,
#18856,#18857,#18858,#18859,#18860,#18861,#18862,#18863,#18864,#18865,#18866,
#18867,#18868,#18869,#18870,#18871,#18872,#18873,#18874,#18875,#18876,#18877,
#18878,#18879,#18880,#18881,#18882,#18883,#18884,#18885,#18886,#18887,#18888,
#18889,#18890,#18891),.UNSPECIFIED.,.F.,.F.,(4,3,3,3,3,3,3,3,3,3,3,3,3,
3,3,3,3,3,3,3,3,3,3,3,3,3,3,3,4),(0.,0.00148924026782088,0.00237768466992155,
0.00240031428091271,0.00307153273081633,0.00357468500117894,0.00360047142136908,
0.00432197233415202,0.00477356764211701,0.00480062856182546,0.0052886236761061,
0.00537382713867274,0.00540070713205367,0.00597487440961069,0.00600078570228188,
0.00645684171980056,0.00657682867032059,0.00660086427251008,0.00704835769063998,
0.00717981783844027,0.00720094284273829,0.00766097488126005,0.00778383982492894,
0.0078010214129665,0.00829799353413678,0.00838897096983562,0.00840109998319471,
0.00899484866798042,0.00960125712365109),.UNSPECIFIED.);
#2709=B_SPLINE_CURVE_WITH_KNOTS('',3,(#18895,#18896,#18897,#18898,#18899,
#18900,#18901,#18902,#18903,#18904,#18905,#18906,#18907,#18908,#18909,#18910,
#18911,#18912,#18913,#18914,#18915,#18916,#18917,#18918,#18919,#18920,#18921,
#18922,#18923,#18924,#18925,#18926,#18927,#18928,#18929,#18930,#18931,#18932,
#18933,#18934,#18935,#18936,#18937,#18938,#18939,#18940,#18941,#18942,#18943,
#18944,#18945,#18946,#18947,#18948,#18949,#18950,#18951,#18952,#18953,#18954,
#18955,#18956,#18957,#18958,#18959,#18960,#18961,#18962,#18963,#18964,#18965,
#18966,#18967,#18968,#18969,#18970,#18971,#18972,#18973),.UNSPECIFIED.,
 .F.,.F.,(4,3,3,3,3,3,3,3,3,3,3,3,3,3,3,3,3,3,3,3,3,3,3,3,3,3,4),(0.,0.00162299209129682,
0.00263692856163744,0.00264790906062433,0.00395638686476062,0.0039718635909365,
0.00485040334252278,0.00527680482969886,0.00529581812124867,0.00622095880290044,
0.00659932264757816,0.00661977265156084,0.00736112912107425,0.00792503767209058,
0.00794372718187301,0.00841598728205416,0.00858967996918311,0.00860570444702908,
0.00906736572635407,0.00925571685290464,0.00926768171218515,0.00981205664257965,
0.00992324054391518,0.00992965897734122,0.0102427913968407,0.0105469048764859,
0.0105916362424973),.UNSPECIFIED.);
#2710=B_SPLINE_CURVE_WITH_KNOTS('',3,(#18977,#18978,#18979,#18980,#18981,
#18982,#18983,#18984,#18985,#18986,#18987,#18988,#18989,#18990,#18991,#18992,
#18993,#18994,#18995,#18996,#18997,#18998,#18999,#19000,#19001,#19002,#19003,
#19004,#19005,#19006,#19007,#19008,#19009,#19010,#19011,#19012,#19013,#19014,
#19015,#19016,#19017,#19018,#19019,#19020,#19021,#19022,#19023,#19024,#19025,
#19026,#19027,#19028,#19029,#19030,#19031,#19032,#19033,#19034,#19035,#19036,
#19037,#19038,#19039,#19040,#19041,#19042,#19043,#19044,#19045,#19046,#19047,
#19048,#19049,#19050,#19051,#19052),.UNSPECIFIED.,.F.,.F.,(4,3,3,3,3,3,
3,3,3,3,3,3,3,3,3,3,3,3,3,3,3,3,3,3,3,4),(0.,0.000670198241349186,0.000677695014211875,
0.00121178630209164,0.00134039648269837,0.00135448412697922,0.00180065626354447,
0.00201059472404756,0.00202974735023086,0.00248224413502192,0.00268079296539674,
0.00270360746120654,0.00357365374674483,0.00402118944809509,0.00404770698701264,
0.00481431515658267,0.00536158593079343,0.00538862458081481,0.00657578262947852,
0.00670198241349177,0.00672748973794275,0.00773324144018303,0.00804237889619011,
0.0080637281365327,0.00982128266121442,0.0107231718615868),
 .UNSPECIFIED.);
#2711=B_SPLINE_CURVE_WITH_KNOTS('',3,(#19056,#19057,#19058,#19059,#19060,
#19061,#19062,#19063,#19064,#19065,#19066,#19067,#19068,#19069,#19070,#19071,
#19072,#19073,#19074,#19075,#19076,#19077,#19078,#19079,#19080,#19081,#19082,
#19083,#19084,#19085,#19086,#19087,#19088,#19089,#19090,#19091,#19092,#19093,
#19094,#19095,#19096,#19097,#19098,#19099,#19100,#19101,#19102,#19103,#19104,
#19105,#19106,#19107,#19108,#19109,#19110,#19111,#19112,#19113,#19114,#19115,
#19116,#19117,#19118,#19119,#19120,#19121,#19122,#19123,#19124,#19125,#19126,
#19127,#19128,#19129,#19130,#19131,#19132,#19133,#19134,#19135,#19136,#19137),
 .UNSPECIFIED.,.F.,.F.,(4,3,3,3,3,3,3,3,3,3,3,3,3,3,3,3,3,3,3,3,3,3,3,3,
3,3,3,4),(0.,0.000605114434157146,0.000605179022010974,0.000885247097935683,
0.00117911739448651,0.00121035804402195,0.00121482791364224,0.00181553706603292,
0.0018245331714837,0.00233958065100891,0.0024207160880439,0.00243323369215935,
0.00345385281984219,0.00363107413206586,0.00364741411510171,0.00419813513510053,
0.00423625315407683,0.00425306575396225,0.0048414321760878,0.00485798624729432,
0.00592735697734792,0.00605179022010969,0.00606599525117843,0.00700618110877007,
0.00726214826413157,0.00727234538984928,0.00902506970597653,0.00968286435217534),
 .UNSPECIFIED.);
#2712=B_SPLINE_CURVE_WITH_KNOTS('',3,(#19315,#19316,#19317,#19318,#19319,
#19320,#19321,#19322,#19323,#19324,#19325,#19326,#19327),.UNSPECIFIED.,
 .F.,.F.,(4,3,3,3,4),(0.,0.00593450809716826,0.00700067642027143,0.0123164151030575,
0.013971448523345),.UNSPECIFIED.);
#2713=B_SPLINE_CURVE_WITH_KNOTS('',3,(#19334,#19335,#19336,#19337,#19338,
#19339,#19340,#19341,#19342,#19343,#19344,#19345,#19346),.UNSPECIFIED.,
 .F.,.F.,(4,3,3,3,4),(0.,0.00603891432879301,0.00699666903166635,0.0124146814900899,
0.0139660167977673),.UNSPECIFIED.);
#2714=B_SPLINE_CURVE_WITH_KNOTS('',3,(#19351,#19352,#19353,#19354,#19355,
#19356,#19357,#19358,#19359,#19360,#19361,#19362,#19363),.UNSPECIFIED.,
 .F.,.F.,(4,3,3,3,4),(0.,0.00541801249293307,0.00696934776611258,0.0130082622991793,
0.0139660167977673),.UNSPECIFIED.);
#2715=B_SPLINE_CURVE_WITH_KNOTS('',3,(#19367,#19368,#19369,#19370,#19371,
#19372,#19373,#19374,#19375,#19376,#19377,#19378,#19379),.UNSPECIFIED.,
 .F.,.F.,(4,3,3,3,4),(0.,0.0053157386001603,0.00697077210307279,0.0129052800531378,
0.013971448523345),.UNSPECIFIED.);
#2716=B_SPLINE_CURVE_WITH_KNOTS('',3,(#19420,#19421,#19422,#19423,#19424,
#19425,#19426,#19427,#19428,#19429,#19430,#19431,#19432,#19433,#19434,#19435,
#19436,#19437,#19438,#19439,#19440,#19441,#19442,#19443,#19444,#19445,#19446,
#19447,#19448,#19449,#19450,#19451,#19452,#19453,#19454,#19455,#19456,#19457,
#19458,#19459,#19460,#19461,#19462,#19463,#19464,#19465,#19466,#19467,#19468,
#19469,#19470,#19471,#19472,#19473,#19474,#19475,#19476,#19477,#19478,#19479,
#19480,#19481,#19482,#19483,#19484,#19485,#19486,#19487,#19488,#19489,#19490,
#19491,#19492,#19493,#19494,#19495,#19496,#19497,#19498,#19499,#19500,#19501,
#19502,#19503,#19504,#19505,#19506,#19507,#19508,#19509,#19510,#19511,#19512,
#19513,#19514,#19515,#19516,#19517,#19518,#19519,#19520,#19521,#19522,#19523,
#19524,#19525,#19526,#19527,#19528,#19529,#19530,#19531,#19532,#19533,#19534,
#19535,#19536,#19537,#19538,#19539,#19540,#19541,#19542,#19543,#19544,#19545,
#19546,#19547,#19548,#19549,#19550,#19551,#19552,#19553,#19554,#19555,#19556,
#19557,#19558,#19559,#19560,#19561,#19562,#19563,#19564,#19565,#19566,#19567,
#19568,#19569,#19570,#19571,#19572,#19573,#19574,#19575,#19576,#19577,#19578,
#19579,#19580,#19581,#19582,#19583,#19584,#19585,#19586,#19587,#19588,#19589,
#19590,#19591,#19592,#19593,#19594,#19595,#19596,#19597,#19598,#19599,#19600,
#19601,#19602,#19603,#19604,#19605,#19606),.UNSPECIFIED.,.F.,.F.,(4,3,3,
3,3,3,3,3,3,3,3,3,3,3,3,3,3,3,3,3,3,3,3,3,3,3,3,3,3,3,3,3,3,3,3,3,3,3,3,
3,3,3,3,3,3,3,3,3,3,3,3,3,3,3,3,3,3,3,3,3,3,3,4),(0.,0.00587025320007918,
0.0116518546601385,0.0124067934665253,0.0183726143829322,0.0233037093202769,
0.0248010444153625,0.0295885380214569,0.0309984330353837,0.0340966058158951,
0.0349555639804154,0.0371915812225473,0.0403989156402141,0.0433496499595692,
0.0463626041882065,0.0466074186405539,0.0494544320203084,0.0524333459706231,
0.0550366402357578,0.0554984816373034,0.0579397193509546,0.0582592733006924,
0.0584943899774514,0.0599505386907733,0.061172236965727,0.0614676725037751,
0.0640852006307616,0.0658681747284104,0.0673052831346648,0.0689343749062278,
0.0699111279608308,0.0713812569705216,0.0728240916258654,0.0729716565715825,
0.0742805734583827,0.0743570049207453,0.0752543696820683,0.0757282061389937,
0.0757370552909,0.0770136999145674,0.0782658534763903,0.078425373133182,
0.0796206612496676,0.0807923001995203,0.0810574254483178,0.0815629826209692,
0.0824911078995598,0.0833977842265763,0.0836193892491146,0.0843234661370702,
0.0844759462860038,0.0848705439497409,0.0859257149372498,0.086104607404437,
0.0871304018360168,0.0873889099510384,0.0884643762089035,0.088522473736195,
0.0895492139112199,0.090301873616073,0.0908732155466535,0.0920722709326854,
0.0932148372811076),.UNSPECIFIED.);
#2717=B_SPLINE_CURVE_WITH_KNOTS('',3,(#19644,#19645,#19646,#19647,#19648,
#19649,#19650,#19651,#19652,#19653,#19654,#19655,#19656,#19657,#19658,#19659,
#19660,#19661,#19662,#19663,#19664,#19665,#19666,#19667,#19668,#19669,#19670,
#19671,#19672,#19673,#19674,#19675,#19676,#19677,#19678,#19679,#19680,#19681,
#19682,#19683,#19684,#19685,#19686,#19687,#19688,#19689,#19690,#19691,#19692,
#19693,#19694,#19695,#19696,#19697,#19698,#19699,#19700,#19701,#19702,#19703,
#19704,#19705,#19706,#19707,#19708,#19709,#19710,#19711,#19712,#19713,#19714,
#19715,#19716,#19717,#19718,#19719,#19720,#19721,#19722,#19723,#19724,#19725,
#19726,#19727,#19728,#19729,#19730,#19731,#19732,#19733,#19734,#19735,#19736,
#19737,#19738,#19739,#19740,#19741,#19742,#19743,#19744,#19745,#19746,#19747,
#19748,#19749,#19750,#19751,#19752,#19753,#19754,#19755,#19756,#19757,#19758,
#19759,#19760,#19761,#19762,#19763,#19764,#19765,#19766,#19767,#19768,#19769,
#19770,#19771,#19772,#19773,#19774,#19775,#19776,#19777,#19778,#19779,#19780,
#19781,#19782,#19783,#19784,#19785,#19786,#19787,#19788,#19789,#19790,#19791,
#19792,#19793,#19794,#19795,#19796,#19797,#19798,#19799,#19800,#19801,#19802,
#19803,#19804,#19805,#19806,#19807,#19808,#19809,#19810,#19811,#19812,#19813,
#19814,#19815,#19816,#19817,#19818,#19819,#19820,#19821,#19822,#19823,#19824,
#19825,#19826,#19827,#19828,#19829,#19830),.UNSPECIFIED.,.F.,.F.,(4,3,3,
3,3,3,3,3,3,3,3,3,3,3,3,3,3,3,3,3,3,3,3,3,3,3,3,3,3,3,3,3,3,3,3,3,3,3,3,
3,3,3,3,3,3,3,3,3,3,3,3,3,3,3,3,3,3,3,3,3,3,3,4),(0.,0.00168391674505757,
0.00237866390505105,0.00293859235176183,0.00392909082463944,0.0047678693047076,
0.00577089595024222,0.00587718470352366,0.00685631905067378,0.00718456765064988,
0.00819626039443761,0.00842377784738116,0.00881577705528549,0.00950100003084725,
0.00968505491475855,0.0106440947494542,0.0116246591280183,0.0117543694070473,
0.0122680279762595,0.0134378823703446,0.0146316209443968,0.0149229678789823,
0.0161755629485317,0.0174530362991548,0.017631554110571,0.0176440794628084,
0.0186861278612264,0.0197665482378735,0.0204254346324111,0.0205701464623328,
0.0220460475716861,0.0235087388140946,0.0251467849670831,0.0261425175891422,
0.0279375140065151,0.0293859235176182,0.0318501667428229,0.0320309300779326,
0.03232451586938,0.0338634522140821,0.0350299832043033,0.0352631082211418,
0.0377194721447005,0.038053160253964,0.0406723517879835,0.0411402929246654,
0.0441530333501108,0.0470174776281889,0.0503147296734146,0.0528946623317125,
0.0558332546834742,0.0565308287838465,0.058771847035236,0.0596542791909667,
0.0627782764692264,0.0673012378967113,0.0690245424335766,0.0705262164422831,
0.0766202357569545,0.0815216901295768,0.0822805858493302,0.0882122169901371,
0.0940349552563772),.UNSPECIFIED.);
#2718=B_SPLINE_CURVE_WITH_KNOTS('',3,(#19849,#19850,#19851,#19852,#19853,
#19854,#19855,#19856,#19857,#19858,#19859,#19860,#19861,#19862,#19863,#19864,
#19865,#19866,#19867,#19868,#19869,#19870,#19871,#19872,#19873,#19874,#19875,
#19876,#19877,#19878,#19879,#19880,#19881,#19882,#19883,#19884,#19885,#19886,
#19887,#19888,#19889,#19890,#19891,#19892,#19893,#19894,#19895,#19896,#19897,
#19898,#19899,#19900,#19901,#19902,#19903,#19904,#19905,#19906,#19907,#19908,
#19909,#19910,#19911,#19912,#19913,#19914,#19915,#19916,#19917,#19918,#19919,
#19920,#19921,#19922,#19923,#19924,#19925,#19926,#19927,#19928,#19929,#19930,
#19931,#19932,#19933,#19934,#19935,#19936,#19937,#19938,#19939,#19940,#19941,
#19942,#19943,#19944,#19945,#19946,#19947,#19948,#19949,#19950,#19951,#19952,
#19953,#19954,#19955,#19956,#19957,#19958,#19959,#19960,#19961,#19962,#19963,
#19964,#19965,#19966,#19967,#19968,#19969,#19970,#19971,#19972,#19973,#19974,
#19975,#19976,#19977,#19978,#19979,#19980,#19981,#19982,#19983,#19984,#19985,
#19986,#19987,#19988,#19989,#19990,#19991,#19992,#19993,#19994,#19995,#19996,
#19997,#19998,#19999,#20000,#20001,#20002,#20003,#20004,#20005,#20006,#20007,
#20008),.UNSPECIFIED.,.F.,.F.,(4,3,3,3,3,3,3,3,3,3,3,3,3,3,3,3,3,3,3,3,
3,3,3,3,3,3,3,3,3,3,3,3,3,3,3,3,3,3,3,3,3,3,3,3,3,3,3,3,3,3,3,3,3,4),(-0.000127168002647682,
0.0032648289235308,0.00665682584970928,0.0119915127057078,0.0134408197020662,
0.0188458139836385,0.0242646482811836,0.0270088074067802,0.032366450211239,
0.0378110333624812,0.0431549242683411,0.0486498535422746,0.054144782816208,
0.0569376853771792,0.0597304018657013,0.060928776668565,0.0662521320816813,
0.0677127705209219,0.0730721047226204,0.0784500787856439,0.0812807582256359,
0.0865149639112802,0.0919904063422261,0.097220456464211,0.10244317541172,
0.107651997921374,0.108416733635064,0.113371574709032,0.115200727487421,
0.118592724413599,0.121984721339778,0.127208398995741,0.132456188050085,
0.135552709044492,0.140533925728601,0.145518391259785,0.150501381841558,
0.155479367307953,0.160446076154363,0.16268868445392,0.166080681380098,
0.169472678306277,0.174505619188982,0.176256672158634,0.181130495805333,
0.186006141113962,0.189824659863348,0.194381555892116,0.198912300408802,
0.203392647568062,0.207549698275247,0.2116829215882,0.215777089793746,0.216960635272776),
 .UNSPECIFIED.);
#2719=B_SPLINE_CURVE_WITH_KNOTS('',3,(#20027,#20028,#20029,#20030,#20031,
#20032,#20033,#20034,#20035,#20036,#20037,#20038,#20039,#20040,#20041,#20042,
#20043,#20044,#20045,#20046,#20047,#20048,#20049,#20050,#20051,#20052,#20053,
#20054,#20055,#20056,#20057,#20058,#20059,#20060,#20061,#20062,#20063,#20064,
#20065,#20066,#20067,#20068,#20069,#20070,#20071,#20072,#20073,#20074,#20075,
#20076,#20077,#20078,#20079,#20080,#20081,#20082,#20083,#20084,#20085,#20086,
#20087,#20088,#20089,#20090,#20091,#20092,#20093,#20094,#20095,#20096,#20097,
#20098,#20099,#20100,#20101,#20102,#20103,#20104,#20105,#20106,#20107,#20108,
#20109,#20110,#20111,#20112,#20113,#20114,#20115,#20116,#20117,#20118,#20119,
#20120,#20121,#20122,#20123,#20124,#20125,#20126,#20127,#20128,#20129,#20130,
#20131,#20132,#20133,#20134,#20135,#20136,#20137,#20138,#20139,#20140,#20141,
#20142,#20143,#20144,#20145,#20146,#20147,#20148,#20149,#20150,#20151,#20152,
#20153,#20154,#20155,#20156,#20157,#20158,#20159,#20160,#20161,#20162,#20163,
#20164,#20165,#20166,#20167,#20168,#20169,#20170,#20171,#20172,#20173,#20174,
#20175,#20176,#20177,#20178,#20179,#20180,#20181,#20182,#20183,#20184,#20185,
#20186,#20187,#20188,#20189,#20190,#20191,#20192,#20193,#20194,#20195),
 .UNSPECIFIED.,.F.,.F.,(4,3,3,3,3,3,3,3,3,3,3,3,3,3,3,3,3,3,3,3,3,3,3,3,
3,3,3,3,3,3,3,3,3,3,3,3,3,3,3,3,3,3,3,3,3,3,3,3,3,3,3,3,3,3,3,3,4),(0.,
0.00406840368139733,0.00816351919635245,0.0122918771767106,0.0134587152954293,
0.0179460716513004,0.0224622816851354,0.0269174305908586,0.0317525397182155,
0.0365884572360659,0.0403761458862878,0.045368531251652,0.0471055035340025,
0.0504701823578598,0.0538348611817171,0.0587609520050433,0.0636963883693916,
0.0686402778496681,0.0735849222481519,0.0785263152925298,0.0807522917725757,
0.08596015285935,0.0911453435853751,0.094211007068005,0.0975756858918623,
0.10094036471572,0.105855287543985,0.107669722363434,0.11283784848067,0.118275174599076,
0.123466116913776,0.128659259968161,0.133850907694542,0.134587152954293,
0.139923299838746,0.145242088010254,0.148045868249722,0.153326319753184,
0.154775225897437,0.157545654220975,0.160316002582348,0.161504583545151,
0.166777046688815,0.172188288550613,0.177494625650974,0.182958319893492,
0.18842201413601,0.193798089195622,0.199161558644946,0.201880729431439,
0.207172416254997,0.208610087079154,0.211974765903011,0.21365710531494,
0.214498275020904,0.215258241940824,0.215339444726868),.UNSPECIFIED.);
#2720=B_SPLINE_CURVE_WITH_KNOTS('',3,(#20797,#20798,#20799,#20800,#20801,
#20802,#20803,#20804,#20805,#20806),.UNSPECIFIED.,.F.,.F.,(4,3,3,4),(0.,
0.00768746870294856,0.0143567530216925,0.0153546747867968),
 .UNSPECIFIED.);
#2721=B_SPLINE_CURVE_WITH_KNOTS('',3,(#20810,#20811,#20812,#20813,#20814,
#20815,#20816,#20817,#20818,#20819),.UNSPECIFIED.,.F.,.F.,(4,3,3,4),(0.,
0.00768475212022721,0.0144698745656401,0.0153509945442703),
 .UNSPECIFIED.);
#2722=B_SPLINE_CURVE_WITH_KNOTS('',3,(#20824,#20825,#20826,#20827,#20828,
#20829,#20830,#20831,#20832,#20833),.UNSPECIFIED.,.F.,.F.,(4,3,3,4),(0.,
0.00678512276816754,0.00766624242405213,0.0153509945442702),
 .UNSPECIFIED.);
#2723=B_SPLINE_CURVE_WITH_KNOTS('',3,(#20840,#20841,#20842,#20843,#20844,
#20845,#20846,#20847,#20848,#20849),.UNSPECIFIED.,.F.,.F.,(4,3,3,4),(0.,
0.00666928397116938,0.00766720608384747,0.0153546747867968),
 .UNSPECIFIED.);
#2724=B_SPLINE_CURVE_WITH_KNOTS('',3,(#20887,#20888,#20889,#20890,#20891,
#20892,#20893,#20894,#20895,#20896,#20897,#20898,#20899,#20900,#20901,#20902,
#20903,#20904,#20905,#20906,#20907,#20908,#20909,#20910,#20911,#20912,#20913,
#20914,#20915,#20916,#20917,#20918,#20919,#20920,#20921,#20922,#20923,#20924,
#20925,#20926,#20927,#20928,#20929,#20930,#20931,#20932,#20933,#20934,#20935,
#20936,#20937,#20938,#20939,#20940,#20941,#20942,#20943,#20944,#20945,#20946,
#20947,#20948,#20949,#20950,#20951,#20952,#20953,#20954,#20955,#20956,#20957,
#20958,#20959,#20960,#20961,#20962,#20963,#20964,#20965,#20966,#20967,#20968,
#20969,#20970,#20971,#20972,#20973,#20974,#20975,#20976,#20977,#20978,#20979,
#20980,#20981,#20982,#20983,#20984,#20985,#20986,#20987,#20988,#20989,#20990,
#20991,#20992,#20993,#20994,#20995,#20996,#20997,#20998,#20999,#21000,#21001,
#21002,#21003,#21004,#21005,#21006,#21007,#21008,#21009,#21010,#21011,#21012,
#21013,#21014,#21015,#21016,#21017,#21018,#21019,#21020,#21021,#21022,#21023,
#21024,#21025,#21026,#21027,#21028,#21029,#21030,#21031,#21032,#21033,#21034,
#21035,#21036,#21037,#21038,#21039,#21040,#21041,#21042,#21043,#21044,#21045,
#21046,#21047,#21048,#21049,#21050,#21051,#21052,#21053,#21054,#21055,#21056,
#21057,#21058,#21059,#21060,#21061,#21062,#21063,#21064,#21065,#21066,#21067,
#21068,#21069,#21070,#21071,#21072,#21073,#21074,#21075,#21076,#21077,#21078,
#21079,#21080,#21081,#21082,#21083,#21084,#21085,#21086,#21087,#21088,#21089,
#21090,#21091,#21092,#21093,#21094,#21095,#21096,#21097,#21098,#21099,#21100),
 .UNSPECIFIED.,.F.,.F.,(4,3,3,3,3,3,3,3,3,3,3,3,3,3,3,3,3,3,3,3,3,3,3,3,
3,3,3,3,3,3,3,3,3,3,3,3,3,3,3,3,3,3,3,3,3,3,3,3,3,3,3,3,3,3,3,3,3,3,3,3,
3,3,3,3,3,3,3,3,3,3,3,4),(0.,0.00536121649079707,0.0107224329815941,0.0119083296245285,
0.0171328352185017,0.0214448659631883,0.023821656300005,0.0294153766011437,
0.0297871200699058,0.0321672989447824,0.0327728648551297,0.0347384176644012,
0.0357560767551434,0.0375285154355795,0.0407799405573036,0.0416735983164754,
0.0428897319263765,0.0456004412105126,0.0475140698351893,0.0500261971384477,
0.0524766748734367,0.0532652736795232,0.0536121649079707,0.0557751307553522,
0.0561021069505934,0.0562927731533692,0.057486465730024,0.0585814667716182,
0.0589040071999902,0.0589733813987678,0.0605030839512922,0.0620069983779697,
0.0634735651758426,0.0643313047141251,0.0643345978895649,0.0656393520467414,
0.0668590262243249,0.0669441062039179,0.0681025607846875,0.0692316257315129,
0.0694789204759748,0.0696958143803621,0.0706207191542974,0.0707145367732808,
0.071381438865015,0.0719262439017434,0.0723764226257606,0.0732437734129232,
0.0740922211334398,0.0742679843726784,0.0750570308711592,0.0757816961429912,
0.0764916855102009,0.0771716653451038,0.0777376391165577,0.0783385807347774,
0.0785857570505588,0.079077943239257,0.0795801179446465,0.0804182473619563,
0.0805402186897528,0.0811493850872042,0.0817226935636484,0.0817585514846556,
0.0821582857848663,0.0823614354785218,0.0827531485315508,0.0830988556073549,
0.0839616629033724,0.0840870494218764,0.0849332566373149,0.0857794638527535),
 .UNSPECIFIED.);
#2725=B_SPLINE_CURVE_WITH_KNOTS('',3,(#21138,#21139,#21140,#21141,#21142,
#21143,#21144,#21145,#21146,#21147,#21148,#21149,#21150,#21151,#21152,#21153,
#21154,#21155,#21156,#21157,#21158,#21159,#21160,#21161,#21162,#21163,#21164,
#21165,#21166,#21167,#21168,#21169,#21170,#21171,#21172,#21173,#21174,#21175,
#21176,#21177,#21178,#21179,#21180,#21181,#21182,#21183,#21184,#21185,#21186,
#21187,#21188,#21189,#21190,#21191,#21192,#21193,#21194,#21195,#21196,#21197,
#21198,#21199,#21200,#21201,#21202,#21203,#21204,#21205,#21206,#21207,#21208,
#21209,#21210,#21211,#21212,#21213,#21214,#21215,#21216,#21217,#21218,#21219,
#21220,#21221,#21222,#21223,#21224,#21225,#21226,#21227,#21228,#21229,#21230,
#21231,#21232,#21233,#21234,#21235,#21236,#21237,#21238,#21239,#21240,#21241,
#21242,#21243,#21244,#21245,#21246,#21247,#21248,#21249,#21250,#21251,#21252,
#21253,#21254,#21255,#21256,#21257,#21258,#21259,#21260,#21261,#21262,#21263,
#21264,#21265,#21266,#21267,#21268,#21269,#21270,#21271,#21272,#21273,#21274,
#21275,#21276,#21277,#21278,#21279,#21280,#21281,#21282,#21283,#21284,#21285,
#21286,#21287,#21288,#21289,#21290,#21291,#21292,#21293,#21294,#21295,#21296,
#21297,#21298,#21299,#21300,#21301,#21302,#21303,#21304,#21305,#21306,#21307,
#21308,#21309,#21310,#21311,#21312,#21313,#21314,#21315,#21316,#21317,#21318,
#21319,#21320,#21321,#21322,#21323,#21324,#21325,#21326,#21327,#21328,#21329,
#21330,#21331,#21332,#21333,#21334,#21335,#21336,#21337,#21338,#21339,#21340,
#21341,#21342,#21343,#21344,#21345,#21346,#21347,#21348,#21349,#21350,#21351,
#21352,#21353,#21354,#21355,#21356,#21357),.UNSPECIFIED.,.F.,.F.,(4,3,3,
3,3,3,3,3,3,3,3,3,3,3,3,3,3,3,3,3,3,3,3,3,3,3,3,3,3,3,3,3,3,3,3,3,3,3,3,
3,3,3,3,3,3,3,3,3,3,3,3,3,3,3,3,3,3,3,3,3,3,3,3,3,3,3,3,3,3,3,3,3,3,4),
(0.,0.000853445909658264,0.00170689181931653,0.00259346888277001,0.00270665419813819,
0.00301811004639099,0.00333278452805475,0.00338331774767277,0.00344497246138023,
0.00398704071753636,0.00405998129720734,0.00463779416072756,0.00522550383422844,
0.00528398471737718,0.00541330839627647,0.00606201299034083,0.00625331267443975,
0.00672179483998648,0.00676663549534561,0.0072193854254239,0.00725603039386378,
0.00783136218365323,0.00811996259441475,0.00880198401199615,0.00936886062699102,
0.010097738709772,0.010826616792553,0.0116132146110347,0.0124664243712336,
0.0133388490992226,0.0135332709906913,0.0139769232258912,0.0147311255351362,
0.0155210222042751,0.0162399251888296,0.0164490515806184,0.0175977301617576,
0.018775784239765,0.0190105677891651,0.0202542001113586,0.021529561127787,
0.0216498696665422,0.0216532335851062,0.0231400660109318,0.0246515136906535,
0.026202452748715,0.0270665419813828,0.0271300556873131,0.0283504938641854,
0.0296458787879955,0.0299579832896972,0.0315284258663565,0.0324798503776594,
0.0328253367756621,0.0352876648060489,0.0378107290799157,0.0386378143164369,
0.0413659622149544,0.0433064671702126,0.0445421276507487,0.0478144982641544,
0.0487197755664892,0.0505253151863032,0.0525549549009522,0.0535380477420698,
0.0541330839627658,0.0565496900761665,0.0625677704660161,0.0649597007553191,
0.0702926004909309,0.074590333644314,0.0757863175478723,0.0811996259441489,
0.0866129343404255),.UNSPECIFIED.);
#2726=B_SPLINE_CURVE_WITH_KNOTS('',3,(#21376,#21377,#21378,#21379,#21380,
#21381,#21382,#21383,#21384,#21385,#21386,#21387,#21388,#21389,#21390,#21391,
#21392,#21393,#21394,#21395,#21396,#21397,#21398,#21399,#21400,#21401,#21402,
#21403,#21404,#21405,#21406,#21407,#21408,#21409,#21410,#21411,#21412,#21413,
#21414,#21415,#21416,#21417,#21418,#21419,#21420,#21421,#21422,#21423,#21424,
#21425,#21426,#21427,#21428,#21429,#21430,#21431,#21432,#21433,#21434,#21435,
#21436,#21437,#21438,#21439,#21440,#21441,#21442,#21443,#21444,#21445,#21446,
#21447,#21448,#21449,#21450,#21451,#21452,#21453,#21454,#21455,#21456,#21457,
#21458,#21459,#21460,#21461,#21462,#21463,#21464,#21465,#21466,#21467,#21468,
#21469,#21470,#21471,#21472,#21473,#21474,#21475,#21476,#21477,#21478,#21479,
#21480,#21481,#21482,#21483,#21484,#21485,#21486,#21487,#21488,#21489,#21490,
#21491,#21492,#21493,#21494,#21495,#21496,#21497,#21498,#21499,#21500,#21501,
#21502,#21503,#21504,#21505,#21506,#21507,#21508,#21509,#21510,#21511,#21512,
#21513,#21514,#21515,#21516,#21517,#21518,#21519,#21520,#21521,#21522,#21523,
#21524,#21525,#21526,#21527,#21528,#21529,#21530,#21531,#21532,#21533,#21534,
#21535),.UNSPECIFIED.,.F.,.F.,(4,3,3,3,3,3,3,3,3,3,3,3,3,3,3,3,3,3,3,3,
3,3,3,3,3,3,3,3,3,3,3,3,3,3,3,3,3,3,3,3,3,3,3,3,3,3,3,3,3,3,3,3,3,4),(-0.000120027570413996,
0.000615336899055743,0.000687456171051644,0.00149493991251728,0.00310990739544856,
0.00633984236131111,0.0117875786308091,0.0127997122930362,0.0183066990136958,
0.0238261998769249,0.0257194521564864,0.0311821835538968,0.0366419530942659,
0.0420953213199303,0.047533539491917,0.0515589318833868,0.0543422828863298,
0.0571261530475139,0.0580188018151119,0.0634547853277745,0.0644786717468369,
0.0699590715687213,0.0754632038688581,0.0773984116102871,0.082796947367055,
0.0882065425473555,0.093617986808073,0.0990281989987573,0.103237891337187,
0.108426657628614,0.109697761268913,0.114131103460074,0.116157631200638,
0.12158252459318,0.127045744727309,0.129077371064088,0.134327451696826,
0.139602688665655,0.144887922475877,0.150186447600716,0.154916850790988,
0.158146785756851,0.161376720722713,0.166713805339851,0.167836590654438,
0.173045937956705,0.178283075697025,0.180756330517889,0.185492323643426,
0.190221955891824,0.194930033223942,0.199617768703279,0.204265609697008,
0.206595810244789),.UNSPECIFIED.);
#2727=B_SPLINE_CURVE_WITH_KNOTS('',3,(#21554,#21555,#21556,#21557,#21558,
#21559,#21560,#21561,#21562,#21563,#21564,#21565,#21566,#21567,#21568,#21569,
#21570,#21571,#21572,#21573,#21574,#21575,#21576,#21577,#21578,#21579,#21580,
#21581,#21582,#21583,#21584,#21585,#21586,#21587,#21588,#21589,#21590,#21591,
#21592,#21593,#21594,#21595,#21596,#21597,#21598,#21599,#21600,#21601,#21602,
#21603,#21604,#21605,#21606,#21607,#21608,#21609,#21610,#21611,#21612,#21613,
#21614,#21615,#21616,#21617,#21618,#21619,#21620,#21621,#21622,#21623,#21624,
#21625,#21626,#21627,#21628,#21629,#21630,#21631,#21632,#21633,#21634,#21635,
#21636,#21637,#21638,#21639,#21640,#21641,#21642,#21643,#21644,#21645,#21646,
#21647,#21648,#21649,#21650,#21651,#21652,#21653,#21654,#21655,#21656,#21657,
#21658,#21659,#21660,#21661,#21662,#21663,#21664,#21665,#21666,#21667,#21668,
#21669,#21670,#21671,#21672,#21673,#21674,#21675,#21676,#21677,#21678,#21679,
#21680,#21681,#21682,#21683,#21684,#21685,#21686,#21687,#21688,#21689,#21690,
#21691,#21692,#21693,#21694,#21695,#21696,#21697,#21698,#21699,#21700,#21701,
#21702,#21703,#21704,#21705,#21706,#21707,#21708,#21709,#21710),
 .UNSPECIFIED.,.F.,.F.,(4,3,3,3,3,3,3,3,3,3,3,3,3,3,3,3,3,3,3,3,3,3,3,3,
3,3,3,3,3,3,3,3,3,3,3,3,3,3,3,3,3,3,3,3,3,3,3,3,3,3,3,3,4),(0.,0.00465397512833474,
0.00934040158699275,0.0140625542141266,0.018797111658081,0.0235416623819038,
0.0258869012718253,0.031135724540156,0.0363582137350459,0.0388303519077379,
0.0441772368004237,0.0453020772256943,0.0485379398846724,0.0517738025436506,
0.0570839432831096,0.0623818493210589,0.0676692441431062,0.0729362028776467,
0.077660703815476,0.0831369521944653,0.088575287007654,0.0906041544513887,
0.0950460719179827,0.0970758797693451,0.102274172320935,0.103547605087301,
0.108966084914322,0.114387970814243,0.119807746002882,0.125219596524798,
0.129434506359127,0.134950329489426,0.140442991021434,0.14237795699504,
0.14782392405742,0.148849682312996,0.151638804562009,0.154427199116194,
0.155321407630952,0.160764764129599,0.166227213607188,0.171695920134864,
0.177169105885651,0.181208308902778,0.186738565261515,0.192256964824344,
0.194151759538691,0.199609501606606,0.200623484856647,0.203859347515625,
0.205477278845114,0.206286244509859,0.207095210174603),.UNSPECIFIED.);
#2728=B_SPLINE_CURVE_WITH_KNOTS('',3,(#22447,#22448,#22449,#22450,#22451,
#22452,#22453,#22454,#22455,#22456,#22457,#22458,#22459,#22460,#22461,#22462,
#22463,#22464,#22465,#22466,#22467,#22468,#22469,#22470,#22471,#22472,#22473,
#22474,#22475,#22476,#22477,#22478,#22479,#22480,#22481,#22482,#22483,#22484,
#22485,#22486,#22487,#22488,#22489,#22490,#22491,#22492,#22493,#22494,#22495,
#22496,#22497,#22498,#22499,#22500,#22501,#22502,#22503,#22504,#22505,#22506,
#22507,#22508,#22509,#22510,#22511,#22512,#22513,#22514,#22515,#22516,#22517,
#22518,#22519,#22520,#22521,#22522,#22523,#22524,#22525,#22526,#22527,#22528,
#22529,#22530,#22531,#22532,#22533,#22534,#22535,#22536,#22537,#22538,#22539,
#22540,#22541,#22542,#22543,#22544,#22545,#22546,#22547,#22548,#22549,#22550,
#22551,#22552),.UNSPECIFIED.,.F.,.F.,(4,3,3,3,3,3,3,3,3,3,3,3,3,3,3,3,3,
3,3,3,3,3,3,3,3,3,3,3,3,3,3,3,3,3,3,4),(0.,0.00197960077599861,0.00247091791055683,
0.00271406396528817,0.00353661742623442,0.00406281433229082,0.00473095927563442,
0.00494183582111366,0.00539811302525832,0.00588176117506153,0.00614016446975763,
0.0064820025407543,0.00670014847819671,0.00703750070456727,0.00735785779192122,
0.00741275373167048,0.00770998130346443,0.00793355713016827,0.00803048320930966,
0.00821222460251388,0.00838031025432408,0.00850817406567731,0.00864821268694884,
0.00877812514044343,0.00890612848419853,0.00902500075932815,0.00903413182795362,
0.00915003699627082,0.00925578338446123,0.00926594216458802,0.00948862534172098,
0.00957480690340761,0.00968337068845401,0.0097292392728174,0.00983010999353415,
0.00988367164222719),.UNSPECIFIED.);
#2729=B_SPLINE_CURVE_WITH_KNOTS('',3,(#22630,#22631,#22632,#22633,#22634,
#22635,#22636,#22637,#22638,#22639,#22640,#22641,#22642,#22643,#22644,#22645,
#22646,#22647,#22648,#22649,#22650,#22651,#22652,#22653,#22654,#22655,#22656,
#22657,#22658,#22659,#22660,#22661,#22662,#22663,#22664,#22665,#22666,#22667,
#22668,#22669,#22670,#22671,#22672,#22673,#22674,#22675,#22676,#22677,#22678,
#22679,#22680,#22681,#22682,#22683,#22684,#22685,#22686,#22687,#22688,#22689,
#22690,#22691,#22692,#22693,#22694,#22695,#22696,#22697,#22698,#22699,#22700,
#22701,#22702,#22703,#22704,#22705,#22706,#22707,#22708,#22709,#22710,#22711,
#22712,#22713,#22714,#22715,#22716,#22717,#22718,#22719,#22720,#22721,#22722,
#22723,#22724,#22725,#22726,#22727,#22728,#22729,#22730,#22731,#22732),
 .UNSPECIFIED.,.F.,.F.,(4,3,3,3,3,3,3,3,3,3,3,3,3,3,3,3,3,3,3,3,3,3,3,3,
3,3,3,3,3,3,3,3,3,3,4),(0.,0.000847545223232314,0.00164832088701133,0.00169509044646463,
0.001942948192431,0.0023393259780218,0.00271143654648364,0.00289047906148623,
0.00324472718726106,0.00339018089292925,0.00373559044008736,0.00380456263483662,
0.00411444755787733,0.00423772611616157,0.00424433990018985,0.00445722296515655,
0.00464735310941275,0.00467010603012326,0.00487822388613578,0.00508527133939388,
0.00526210164977017,0.00543234850501674,0.00546390351830185,0.00560937914391588,
0.00574753034539324,0.00582575793302101,0.0059328165626262,0.00609723736525646,
0.00616149255899438,0.00629753167797226,0.00635658917424234,0.0064781662286767,
0.0066043156769876,0.0067284745812143,0.00678036178585848),
 .UNSPECIFIED.);
#2730=B_SPLINE_CURVE_WITH_KNOTS('',3,(#22746,#22747,#22748,#22749,#22750,
#22751,#22752,#22753,#22754,#22755,#22756,#22757,#22758,#22759,#22760,#22761,
#22762,#22763,#22764,#22765,#22766,#22767,#22768,#22769,#22770,#22771,#22772,
#22773,#22774,#22775,#22776,#22777,#22778,#22779,#22780,#22781,#22782,#22783,
#22784,#22785,#22786,#22787,#22788,#22789,#22790,#22791,#22792,#22793,#22794,
#22795,#22796,#22797,#22798,#22799,#22800,#22801,#22802,#22803,#22804,#22805,
#22806,#22807,#22808,#22809,#22810,#22811,#22812,#22813,#22814,#22815,#22816,
#22817,#22818,#22819,#22820,#22821,#22822,#22823,#22824,#22825,#22826,#22827,
#22828,#22829,#22830,#22831,#22832,#22833,#22834,#22835,#22836,#22837,#22838,
#22839,#22840,#22841,#22842,#22843,#22844,#22845,#22846,#22847,#22848,#22849,
#22850,#22851,#22852,#22853,#22854,#22855,#22856,#22857,#22858,#22859,#22860),
 .UNSPECIFIED.,.F.,.F.,(4,3,3,3,3,3,3,3,3,3,3,3,3,3,3,3,3,3,3,3,3,3,3,3,
3,3,3,3,3,3,3,3,3,3,3,3,3,3,4),(0.,9.18561239655606E-5,0.000187247318122397,
0.000223179866200178,0.000322995769329295,0.000396457195248618,0.000516673504746917,
0.000622443478716646,0.000731484061345082,0.000845574170253623,0.000858929210602675,
0.000978407301811063,0.00110276605193038,0.00123492035522181,0.00124488695743329,
0.00139114459142845,0.00158341591401497,0.00178580066086868,0.00186733043614994,
0.00197093668229903,0.00218794771760141,0.00242197326922363,0.00248977391486658,
0.00258515278144125,0.00295788257484743,0.00321997742071528,0.00365085122472788,
0.00373466087229989,0.00424559974900295,0.00453032492225145,0.0049795478297332,
0.00564687419923879,0.00587646790730166,0.00672137634321008,0.007233651137532,
0.0074693217445998,0.00858965034752487,0.00971088683054975,0.00995909565946641),
 .UNSPECIFIED.);
#2731=B_SPLINE_CURVE_WITH_KNOTS('',3,(#23010,#23011,#23012,#23013,#23014,
#23015,#23016,#23017,#23018,#23019,#23020,#23021,#23022,#23023,#23024,#23025,
#23026,#23027),.UNSPECIFIED.,.F.,.F.,(4,2,2,2,2,2,2,2,4),(0.,0.000517355166269151,
0.0010347103325383,0.00155206549880745,0.0020694206650766,0.00310413099761494,
0.00413884133015328,0.00620826199522997,0.00827768266030667),
 .UNSPECIFIED.);
#2732=B_SPLINE_CURVE_WITH_KNOTS('',3,(#23105,#23106,#23107,#23108,#23109,
#23110,#23111,#23112,#23113,#23114,#23115,#23116,#23117,#23118,#23119,#23120,
#23121,#23122,#23123,#23124,#23125,#23126,#23127,#23128,#23129,#23130,#23131,
#23132,#23133,#23134,#23135,#23136,#23137,#23138,#23139,#23140,#23141,#23142,
#23143,#23144,#23145,#23146,#23147,#23148,#23149,#23150,#23151,#23152,#23153,
#23154,#23155,#23156,#23157,#23158,#23159,#23160,#23161,#23162,#23163,#23164,
#23165,#23166,#23167,#23168,#23169,#23170,#23171,#23172,#23173,#23174,#23175,
#23176,#23177,#23178,#23179,#23180,#23181,#23182,#23183,#23184,#23185,#23186,
#23187,#23188,#23189,#23190,#23191,#23192,#23193,#23194,#23195,#23196,#23197,
#23198,#23199,#23200,#23201,#23202,#23203,#23204,#23205,#23206,#23207,#23208,
#23209,#23210),.UNSPECIFIED.,.F.,.F.,(4,3,3,3,3,3,3,3,3,3,3,3,3,3,3,3,3,
3,3,3,3,3,3,3,3,3,3,3,3,3,3,3,3,3,3,4),(0.,0.00135723929435243,0.00204946145676226,
0.00228622203285677,0.00292292848099983,0.00341673681344062,0.0039067606490192,
0.00409892291352452,0.00448120231546935,0.00453023630184375,0.0049206132320938,
0.00512365364190566,0.00542385726001582,0.00560331504583438,0.00586060524797844,
0.0061050977016897,0.00614838437028681,0.00637684630907044,0.00658758940133999,
0.00660530824785407,0.0066607497344774,0.00681852624425174,0.00696704562612621,
0.00706377833482601,0.00717311509866798,0.00729505291280085,0.00741140394444247,
0.00748396395177441,0.00758472220731649,0.00768548046285857,0.00777764568926981,
0.00785794851170659,0.00794166314495388,0.00803100987111596,0.00811779416605641,
0.00819784582704918),.UNSPECIFIED.);
#2733=B_SPLINE_CURVE_WITH_KNOTS('',3,(#23287,#23288,#23289,#23290,#23291,
#23292,#23293,#23294,#23295,#23296,#23297,#23298,#23299,#23300,#23301,#23302,
#23303,#23304,#23305,#23306,#23307,#23308,#23309,#23310,#23311,#23312,#23313,
#23314,#23315,#23316,#23317,#23318,#23319,#23320,#23321,#23322,#23323,#23324,
#23325,#23326,#23327,#23328,#23329,#23330,#23331,#23332,#23333,#23334,#23335,
#23336,#23337,#23338,#23339,#23340,#23341,#23342,#23343,#23344,#23345,#23346,
#23347,#23348,#23349,#23350,#23351,#23352,#23353,#23354,#23355,#23356,#23357,
#23358,#23359,#23360,#23361,#23362,#23363,#23364,#23365,#23366,#23367,#23368,
#23369,#23370,#23371,#23372,#23373,#23374,#23375,#23376,#23377,#23378,#23379,
#23380,#23381,#23382,#23383),.UNSPECIFIED.,.F.,.F.,(4,3,3,3,3,3,3,3,3,3,
3,3,3,3,3,3,3,3,3,3,3,3,3,3,3,3,3,3,3,3,3,3,4),(0.,0.000170769119259004,
0.000305904332796239,0.000426640701961217,0.000599187316529111,0.00062182697372188,
0.000756823578195052,0.000853281403922433,0.000962782991909417,0.00113222926114292,
0.00127992210588365,0.001328896990288,0.00148406066630655,0.00164727023196531,
0.00170656280784487,0.00171810399452786,0.00194497343526638,0.00212783935765393,
0.00237961725595501,0.00255603792528681,0.00255984421176727,0.0027868478112769,
0.00299980946583919,0.00330293529271853,0.00341312561568967,0.00377553104277187,
0.00392002161607634,0.00428886752640719,0.00468125453704979,0.00487455036175816,
0.00511968842353449,0.0061218062232531,0.00682625123137931),
 .UNSPECIFIED.);
#2734=B_SPLINE_CURVE_WITH_KNOTS('',3,(#23387,#23388,#23389,#23390,#23391,
#23392,#23393,#23394,#23395,#23396,#23397,#23398,#23399,#23400,#23401,#23402,
#23403,#23404,#23405,#23406,#23407,#23408,#23409,#23410,#23411,#23412,#23413,
#23414,#23415,#23416,#23417,#23418,#23419,#23420,#23421,#23422,#23423,#23424,
#23425,#23426,#23427,#23428,#23429,#23430,#23431,#23432,#23433,#23434,#23435,
#23436,#23437,#23438,#23439,#23440,#23441,#23442,#23443,#23444,#23445,#23446,
#23447,#23448,#23449,#23450,#23451,#23452,#23453,#23454,#23455,#23456,#23457,
#23458,#23459,#23460,#23461,#23462,#23463,#23464,#23465,#23466,#23467,#23468,
#23469,#23470,#23471,#23472,#23473,#23474,#23475,#23476,#23477,#23478,#23479,
#23480,#23481,#23482,#23483,#23484,#23485,#23486,#23487,#23488,#23489,#23490,
#23491,#23492),.UNSPECIFIED.,.F.,.F.,(4,3,3,3,3,3,3,3,3,3,3,3,3,3,3,3,3,
3,3,3,3,3,3,3,3,3,3,3,3,3,3,3,3,3,3,4),(0.,0.00197960077597682,0.00247091791055683,
0.00271406396528818,0.00353661742623437,0.00406281433229082,0.00473095927563172,
0.00494183582111366,0.00539811302525833,0.0058817611750583,0.00614016446975659,
0.00648200254113197,0.00670014847819671,0.00703750070456741,0.00735785779192378,
0.00741275373167048,0.00770998130346427,0.00793355713016827,0.00803048320930966,
0.00821222460251474,0.0083803102543245,0.00850817406567731,0.00864821268694884,
0.00877812514044313,0.00890612848419838,0.00902500075932787,0.00903413182795362,
0.00915003699627082,0.00925578338446087,0.00926594216458802,0.00948862534172096,
0.00957480690340761,0.00968337068845101,0.0097292392728174,0.00983010999353228,
0.00988367164222719),.UNSPECIFIED.);
#2735=B_SPLINE_CURVE_WITH_KNOTS('',3,(#23635,#23636,#23637,#23638,#23639,
#23640,#23641,#23642,#23643,#23644,#23645,#23646,#23647,#23648,#23649,#23650,
#23651,#23652,#23653,#23654,#23655,#23656,#23657,#23658,#23659,#23660,#23661,
#23662,#23663,#23664,#23665,#23666,#23667,#23668,#23669,#23670,#23671,#23672,
#23673,#23674,#23675,#23676,#23677,#23678,#23679,#23680,#23681,#23682,#23683,
#23684,#23685,#23686,#23687,#23688,#23689,#23690,#23691,#23692,#23693,#23694,
#23695,#23696,#23697,#23698,#23699,#23700,#23701,#23702,#23703,#23704,#23705,
#23706,#23707,#23708,#23709,#23710,#23711,#23712,#23713,#23714,#23715,#23716,
#23717,#23718,#23719,#23720,#23721,#23722,#23723,#23724,#23725,#23726,#23727,
#23728,#23729,#23730,#23731,#23732,#23733,#23734,#23735,#23736,#23737,#23738,
#23739,#23740,#23741,#23742,#23743,#23744,#23745,#23746,#23747,#23748,#23749),
 .UNSPECIFIED.,.F.,.F.,(4,3,3,3,3,3,3,3,3,3,3,3,3,3,3,3,3,3,3,3,3,3,3,3,
3,3,3,3,3,3,3,3,3,3,3,3,3,3,4),(0.,9.18561239650228E-5,0.000187247318121302,
0.000223179866200187,0.000322995769329302,0.000396457195248715,0.000516673504700863,
0.000622443478716646,0.000731484061341045,0.000845574170246189,0.000858929210603472,
0.000978407301793839,0.00110276605189386,0.00123492035516868,0.00124488695743329,
0.00139114459142878,0.00158341591400849,0.0017858006608566,0.00186733043614994,
0.00197093668229905,0.00218794771763813,0.0024219732692966,0.00248977391486658,
0.0025851527814412,0.00295788257505407,0.00321997742071546,0.00365085122470423,
0.00373466087229989,0.00424559974907391,0.00453032492225087,0.0049795478297332,
0.00564687419895804,0.00587646790729939,0.00672137634272312,0.00723365113753139,
0.0074693217445998,0.00858965034915604,0.00971088683381047,0.00995909565946641),
 .UNSPECIFIED.);
#2736=B_SPLINE_CURVE_WITH_KNOTS('',3,(#23846,#23847,#23848,#23849,#23850,
#23851,#23852,#23853,#23854,#23855,#23856,#23857,#23858,#23859,#23860,#23861,
#23862,#23863,#23864,#23865,#23866,#23867,#23868,#23869,#23870,#23871,#23872,
#23873,#23874,#23875,#23876,#23877,#23878,#23879,#23880,#23881,#23882,#23883,
#23884,#23885,#23886,#23887,#23888,#23889,#23890,#23891,#23892,#23893,#23894,
#23895,#23896,#23897,#23898,#23899,#23900,#23901,#23902,#23903,#23904,#23905,
#23906,#23907,#23908,#23909,#23910,#23911,#23912,#23913,#23914,#23915,#23916,
#23917,#23918,#23919,#23920,#23921,#23922,#23923,#23924,#23925,#23926,#23927,
#23928,#23929,#23930,#23931,#23932,#23933,#23934,#23935,#23936,#23937,#23938,
#23939,#23940,#23941,#23942),.UNSPECIFIED.,.F.,.F.,(4,3,3,3,3,3,3,3,3,3,
3,3,3,3,3,3,3,3,3,3,3,3,3,3,3,3,3,3,3,3,3,3,4),(0.,0.00017076911926328,
0.000305904332796252,0.000426640701961203,0.000599187316529732,0.000621826973721879,
0.000756823578194972,0.000853281403922405,0.000962782991909374,0.00113222926114158,
0.00127992210588361,0.00132889699028796,0.00148406066630834,0.0016472702319681,
0.00170656280784481,0.00171810399452776,0.00194497343526742,0.00212783935765386,
0.00237961725595523,0.00255603792528674,0.00255984421176721,0.00278684781127691,
0.00299980946583915,0.00330293529271767,0.00341312561568961,0.00377553104277046,
0.00392002161607631,0.00428886752635139,0.0046812545369514,0.00487455036175753,
0.00511968842353445,0.00612180622110039,0.00682625123137929),
 .UNSPECIFIED.);
#2737=B_SPLINE_CURVE_WITH_KNOTS('',3,(#23950,#23951,#23952,#23953,#23954,
#23955,#23956,#23957,#23958,#23959,#23960,#23961,#23962,#23963,#23964,#23965,
#23966,#23967,#23968,#23969,#23970,#23971,#23972,#23973,#23974,#23975,#23976,
#23977,#23978,#23979,#23980,#23981,#23982,#23983,#23984,#23985,#23986,#23987,
#23988,#23989,#23990,#23991,#23992,#23993,#23994,#23995,#23996,#23997,#23998,
#23999,#24000,#24001,#24002,#24003,#24004,#24005,#24006,#24007,#24008,#24009,
#24010,#24011,#24012,#24013,#24014,#24015,#24016,#24017,#24018,#24019,#24020,
#24021,#24022,#24023,#24024,#24025,#24026,#24027,#24028,#24029,#24030,#24031,
#24032,#24033,#24034,#24035,#24036,#24037,#24038,#24039,#24040,#24041,#24042,
#24043,#24044,#24045,#24046,#24047,#24048,#24049,#24050,#24051,#24052,#24053,
#24054,#24055),.UNSPECIFIED.,.F.,.F.,(4,3,3,3,3,3,3,3,3,3,3,3,3,3,3,3,3,
3,3,3,3,3,3,3,3,3,3,3,3,3,3,3,3,3,3,4),(0.,0.00135723929435243,0.00204946145676226,
0.00228622203285677,0.00292292848099983,0.00341673681344062,0.0039067606490192,
0.00409892291352452,0.00448120231546935,0.00453023630184375,0.0049206132320938,
0.00512365364190566,0.00542385726001582,0.00560331504583438,0.00586060524797844,
0.0061050977016897,0.00614838437028681,0.00637684630907044,0.00658758940133999,
0.00660530824785407,0.0066607497344774,0.00681852624425174,0.00696704562612621,
0.00706377833482601,0.00717311509866798,0.00729505291280085,0.00741140394444247,
0.00748396395177441,0.00758472220731649,0.00768548046285857,0.00777764568926981,
0.00785794851170659,0.00794166314495388,0.00803100987111596,0.00811779416605641,
0.00819784582704918),.UNSPECIFIED.);
#2738=B_SPLINE_CURVE_WITH_KNOTS('',3,(#24202,#24203,#24204,#24205,#24206,
#24207,#24208,#24209,#24210,#24211,#24212,#24213,#24214,#24215,#24216,#24217,
#24218,#24219),.UNSPECIFIED.,.F.,.F.,(4,2,2,2,2,2,2,2,4),(0.,0.000517355166269167,
0.00103471033253833,0.0015520654988075,0.00206942066507667,0.00310413099761498,
0.0041388413301533,0.00620826199522999,0.00827768266030668),
 .UNSPECIFIED.);
#2739=B_SPLINE_CURVE_WITH_KNOTS('',3,(#24292,#24293,#24294,#24295,#24296,
#24297,#24298,#24299,#24300,#24301,#24302,#24303,#24304,#24305,#24306,#24307,
#24308,#24309,#24310,#24311,#24312,#24313,#24314,#24315,#24316,#24317,#24318,
#24319,#24320,#24321,#24322,#24323,#24324,#24325,#24326,#24327,#24328,#24329,
#24330,#24331,#24332,#24333,#24334,#24335,#24336,#24337,#24338,#24339,#24340,
#24341,#24342,#24343,#24344,#24345,#24346,#24347,#24348,#24349,#24350,#24351,
#24352,#24353,#24354,#24355,#24356,#24357,#24358,#24359,#24360,#24361,#24362,
#24363,#24364,#24365,#24366,#24367,#24368,#24369,#24370,#24371,#24372,#24373,
#24374,#24375,#24376,#24377,#24378,#24379,#24380,#24381,#24382,#24383,#24384,
#24385,#24386,#24387,#24388,#24389,#24390,#24391,#24392,#24393,#24394,#24395,
#24396,#24397,#24398,#24399,#24400,#24401,#24402,#24403,#24404,#24405,#24406),
 .UNSPECIFIED.,.F.,.F.,(4,3,3,3,3,3,3,3,3,3,3,3,3,3,3,3,3,3,3,3,3,3,3,3,
3,3,3,3,3,3,3,3,3,3,3,3,3,3,4),(0.,9.18561239650228E-5,0.000187247318121302,
0.000223179866200187,0.000322995769329302,0.000396457195248715,0.000516673504700863,
0.000622443478716646,0.000731484061341045,0.000845574170246189,0.000858929210603472,
0.000978407301793839,0.00110276605189386,0.00123492035516868,0.00124488695743329,
0.00139114459142878,0.00158341591400849,0.0017858006608566,0.00186733043614994,
0.00197093668229905,0.00218794771763813,0.0024219732692966,0.00248977391486658,
0.0025851527814412,0.00295788257505407,0.00321997742071546,0.00365085122470423,
0.00373466087229989,0.00424559974907391,0.00453032492225087,0.0049795478297332,
0.00564687419895804,0.00587646790729939,0.00672137634272312,0.00723365113753139,
0.0074693217445998,0.00858965034915604,0.00971088683381047,0.00995909565946641),
 .UNSPECIFIED.);
#2740=B_SPLINE_CURVE_WITH_KNOTS('',3,(#24410,#24411,#24412,#24413,#24414,
#24415,#24416,#24417,#24418,#24419,#24420,#24421,#24422,#24423,#24424,#24425,
#24426,#24427,#24428,#24429,#24430,#24431,#24432,#24433,#24434,#24435,#24436,
#24437,#24438,#24439,#24440,#24441,#24442,#24443,#24444,#24445,#24446,#24447,
#24448,#24449,#24450,#24451,#24452,#24453,#24454,#24455,#24456,#24457,#24458,
#24459,#24460,#24461,#24462,#24463,#24464,#24465,#24466,#24467,#24468,#24469,
#24470,#24471,#24472,#24473,#24474,#24475,#24476,#24477,#24478,#24479,#24480,
#24481,#24482,#24483,#24484,#24485,#24486,#24487,#24488,#24489,#24490,#24491,
#24492,#24493,#24494,#24495,#24496,#24497,#24498,#24499,#24500,#24501,#24502,
#24503,#24504,#24505,#24506,#24507,#24508,#24509,#24510,#24511,#24512),
 .UNSPECIFIED.,.F.,.F.,(4,3,3,3,3,3,3,3,3,3,3,3,3,3,3,3,3,3,3,3,3,3,3,3,
3,3,3,3,3,3,3,3,3,3,4),(0.,0.000847545223232322,0.00164832088234661,0.00169509044646464,
0.00194294819243123,0.00233932597799748,0.00271143654641038,0.0028904790614833,
0.00324472718723284,0.00339018089292929,0.00373559044000401,0.0038045626348364,
0.00411444755781185,0.00423772611616159,0.0042443399001899,0.00445722296515594,
0.00464735310929138,0.00467010603012198,0.00487822388608553,0.0050852713393939,
0.0052621016497477,0.00543234850496587,0.00546390351830187,0.00560937914397249,
0.00574753034550799,0.00582575793302147,0.0059328165626262,0.00609723736487279,
0.00616149255899418,0.00629753167790733,0.00635658917424235,0.00647816622867606,
0.00660431567688951,0.0067284745810643,0.0067803617858585),
 .UNSPECIFIED.);
#2741=B_SPLINE_CURVE_WITH_KNOTS('',3,(#24654,#24655,#24656,#24657,#24658,
#24659,#24660,#24661,#24662,#24663,#24664,#24665,#24666,#24667,#24668,#24669,
#24670,#24671,#24672,#24673,#24674,#24675,#24676,#24677,#24678,#24679,#24680,
#24681,#24682,#24683,#24684,#24685,#24686,#24687,#24688,#24689,#24690,#24691,
#24692,#24693,#24694,#24695,#24696,#24697,#24698,#24699,#24700,#24701,#24702,
#24703,#24704,#24705,#24706,#24707,#24708,#24709,#24710,#24711,#24712,#24713,
#24714,#24715,#24716,#24717,#24718,#24719,#24720,#24721,#24722,#24723,#24724,
#24725,#24726,#24727,#24728,#24729,#24730,#24731,#24732,#24733,#24734,#24735,
#24736,#24737,#24738,#24739,#24740,#24741,#24742,#24743,#24744,#24745,#24746,
#24747,#24748,#24749,#24750,#24751,#24752,#24753,#24754,#24755,#24756,#24757,
#24758,#24759),.UNSPECIFIED.,.F.,.F.,(4,3,3,3,3,3,3,3,3,3,3,3,3,3,3,3,3,
3,3,3,3,3,3,3,3,3,3,3,3,3,3,3,3,3,3,4),(0.,0.00197960077764265,0.00247091791055683,
0.00271406396528808,0.00353661742634433,0.00406281433229014,0.00473095927595116,
0.00494183582111366,0.00539811302525782,0.0058817611751927,0.00614016447010104,
0.00648200254249054,0.00670014847819659,0.00703750070457104,0.00735785779193372,
0.00741275373167048,0.0077099813035103,0.00793355713016826,0.00803048320930966,
0.00821222460247987,0.00838031025425421,0.00850817406567739,0.00864821268694884,
0.00877812514043141,0.00890612848419257,0.00902500075930251,0.00903413182795372,
0.00915003699627087,0.00925578338446177,0.00926594216458802,0.00948862534172095,
0.00957480690340761,0.00968337068845094,0.0097292392728174,0.00983010999352899,
0.00988367164222719),.UNSPECIFIED.);
#2742=B_SPLINE_CURVE_WITH_KNOTS('',3,(#24840,#24841,#24842,#24843,#24844,
#24845,#24846,#24847,#24848,#24849,#24850,#24851,#24852,#24853,#24854,#24855,
#24856,#24857,#24858,#24859,#24860,#24861,#24862,#24863,#24864,#24865,#24866,
#24867,#24868,#24869,#24870,#24871,#24872,#24873,#24874,#24875,#24876,#24877,
#24878,#24879,#24880,#24881,#24882,#24883,#24884,#24885,#24886,#24887,#24888,
#24889,#24890,#24891,#24892,#24893,#24894,#24895,#24896,#24897,#24898,#24899,
#24900,#24901,#24902,#24903,#24904,#24905,#24906,#24907,#24908,#24909,#24910,
#24911,#24912,#24913,#24914,#24915,#24916,#24917,#24918,#24919,#24920,#24921,
#24922,#24923,#24924,#24925,#24926,#24927,#24928,#24929,#24930,#24931,#24932,
#24933,#24934,#24935,#24936,#24937,#24938,#24939,#24940,#24941,#24942,#24943,
#24944,#24945),.UNSPECIFIED.,.F.,.F.,(4,3,3,3,3,3,3,3,3,3,3,3,3,3,3,3,3,
3,3,3,3,3,3,3,3,3,3,3,3,3,3,3,3,3,3,4),(0.,0.00197960077599861,0.00247091791055683,
0.00271406396528817,0.00353661742623442,0.00406281433229082,0.00473095927563442,
0.00494183582111366,0.00539811302525832,0.00588176117506153,0.00614016446975763,
0.0064820025407543,0.00670014847819671,0.00703750070456727,0.00735785779192122,
0.00741275373167048,0.00770998130346443,0.00793355713016827,0.00803048320930966,
0.00821222460251388,0.00838031025432408,0.00850817406567731,0.00864821268694884,
0.00877812514044343,0.00890612848419853,0.00902500075932815,0.00903413182795362,
0.00915003699627082,0.00925578338446123,0.00926594216458802,0.00948862534172098,
0.00957480690340761,0.00968337068845401,0.0097292392728174,0.00983010999353415,
0.00988367164222719),.UNSPECIFIED.);
#2743=B_SPLINE_CURVE_WITH_KNOTS('',3,(#25016,#25017,#25018,#25019,#25020,
#25021,#25022,#25023,#25024,#25025,#25026,#25027,#25028,#25029,#25030,#25031,
#25032,#25033,#25034,#25035,#25036,#25037,#25038,#25039,#25040,#25041,#25042,
#25043,#25044,#25045,#25046,#25047,#25048,#25049,#25050,#25051,#25052,#25053,
#25054,#25055,#25056,#25057,#25058,#25059,#25060,#25061,#25062,#25063,#25064,
#25065,#25066,#25067,#25068,#25069,#25070,#25071,#25072,#25073,#25074,#25075,
#25076,#25077,#25078,#25079,#25080,#25081,#25082,#25083,#25084,#25085,#25086,
#25087,#25088,#25089,#25090,#25091,#25092,#25093,#25094,#25095,#25096,#25097,
#25098,#25099,#25100,#25101,#25102,#25103,#25104,#25105,#25106,#25107,#25108,
#25109,#25110,#25111,#25112,#25113,#25114,#25115,#25116,#25117,#25118,#25119,
#25120,#25121,#25122,#25123,#25124,#25125,#25126,#25127,#25128,#25129,#25130),
 .UNSPECIFIED.,.F.,.F.,(4,3,3,3,3,3,3,3,3,3,3,3,3,3,3,3,3,3,3,3,3,3,3,3,
3,3,3,3,3,3,3,3,3,3,3,3,3,3,4),(0.,9.18561239655192E-5,0.000187247318122313,
0.000223179866200178,0.000322995769329295,0.000396457195248687,0.000516673504700411,
0.000622443478716646,0.000731484061341489,0.000845574170246325,0.000858929210603472,
0.000978407301793866,0.0011027660518945,0.0012349203551681,0.00124488695743329,
0.00139114459142878,0.00158341591400812,0.00178580066085747,0.00186733043614994,
0.00197093668229905,0.00218794771764027,0.00242197326929741,0.00248977391486658,
0.0025851527814412,0.00295788257505396,0.00321997742071547,0.00365085122470463,
0.00373466087229989,0.00424559974907373,0.00453032492225088,0.0049795478297332,
0.00564687419896703,0.0058764679072994,0.00672137634272318,0.00723365113753139,
0.0074693217445998,0.00858965034916116,0.00971088683382174,0.00995909565946641),
 .UNSPECIFIED.);
#2744=LINE('',#16758,#3756);
#2745=LINE('',#16820,#3757);
#2746=LINE('',#16823,#3758);
#2747=LINE('',#16831,#3759);
#2748=LINE('',#16834,#3760);
#2749=LINE('',#16840,#3761);
#2750=LINE('',#16843,#3762);
#2751=LINE('',#16892,#3763);
#2752=LINE('',#16897,#3764);
#2753=LINE('',#16902,#3765);
#2754=LINE('',#16907,#3766);
#2755=LINE('',#16912,#3767);
#2756=LINE('',#16917,#3768);
#2757=LINE('',#16922,#3769);
#2758=LINE('',#16927,#3770);
#2759=LINE('',#16932,#3771);
#2760=LINE('',#16937,#3772);
#2761=LINE('',#16942,#3773);
#2762=LINE('',#16947,#3774);
#2763=LINE('',#16949,#3775);
#2764=LINE('',#16954,#3776);
#2765=LINE('',#16962,#3777);
#2766=LINE('',#16965,#3778);
#2767=LINE('',#16970,#3779);
#2768=LINE('',#16976,#3780);
#2769=LINE('',#16982,#3781);
#2770=LINE('',#16988,#3782);
#2771=LINE('',#16995,#3783);
#2772=LINE('',#16998,#3784);
#2773=LINE('',#17352,#3785);
#2774=LINE('',#17354,#3786);
#2775=LINE('',#17362,#3787);
#2776=LINE('',#17367,#3788);
#2777=LINE('',#17370,#3789);
#2778=LINE('',#17372,#3790);
#2779=LINE('',#17374,#3791);
#2780=LINE('',#17877,#3792);
#2781=LINE('',#18128,#3793);
#2782=LINE('',#18379,#3794);
#2783=LINE('',#18550,#3795);
#2784=LINE('',#18632,#3796);
#2785=LINE('',#18722,#3797);
#2786=LINE('',#18805,#3798);
#2787=LINE('',#18975,#3799);
#2788=LINE('',#19138,#3800);
#2789=LINE('',#19142,#3801);
#2790=LINE('',#19144,#3802);
#2791=LINE('',#19146,#3803);
#2792=LINE('',#19148,#3804);
#2793=LINE('',#19150,#3805);
#2794=LINE('',#19151,#3806);
#2795=LINE('',#19155,#3807);
#2796=LINE('',#19157,#3808);
#2797=LINE('',#19159,#3809);
#2798=LINE('',#19161,#3810);
#2799=LINE('',#19162,#3811);
#2800=LINE('',#19164,#3812);
#2801=LINE('',#19168,#3813);
#2802=LINE('',#19171,#3814);
#2803=LINE('',#19172,#3815);
#2804=LINE('',#19174,#3816);
#2805=LINE('',#19178,#3817);
#2806=LINE('',#19181,#3818);
#2807=LINE('',#19183,#3819);
#2808=LINE('',#19184,#3820);
#2809=LINE('',#19187,#3821);
#2810=LINE('',#19189,#3822);
#2811=LINE('',#19191,#3823);
#2812=LINE('',#19193,#3824);
#2813=LINE('',#19195,#3825);
#2814=LINE('',#19196,#3826);
#2815=LINE('',#19198,#3827);
#2816=LINE('',#19202,#3828);
#2817=LINE('',#19205,#3829);
#2818=LINE('',#19207,#3830);
#2819=LINE('',#19211,#3831);
#2820=LINE('',#19219,#3832);
#2821=LINE('',#19229,#3833);
#2822=LINE('',#19237,#3834);
#2823=LINE('',#19251,#3835);
#2824=LINE('',#19255,#3836);
#2825=LINE('',#19259,#3837);
#2826=LINE('',#19263,#3838);
#2827=LINE('',#19267,#3839);
#2828=LINE('',#19271,#3840);
#2829=LINE('',#19275,#3841);
#2830=LINE('',#19279,#3842);
#2831=LINE('',#19283,#3843);
#2832=LINE('',#19288,#3844);
#2833=LINE('',#19290,#3845);
#2834=LINE('',#19294,#3846);
#2835=LINE('',#19298,#3847);
#2836=LINE('',#19299,#3848);
#2837=LINE('',#19303,#3849);
#2838=LINE('',#19306,#3850);
#2839=LINE('',#19307,#3851);
#2840=LINE('',#19310,#3852);
#2841=LINE('',#19312,#3853);
#2842=LINE('',#19313,#3854);
#2843=LINE('',#20730,#3855);
#2844=LINE('',#20739,#3856);
#2845=LINE('',#20749,#3857);
#2846=LINE('',#20758,#3858);
#2847=LINE('',#20767,#3859);
#2848=LINE('',#20769,#3860);
#2849=LINE('',#20773,#3861);
#2850=LINE('',#20775,#3862);
#2851=LINE('',#20777,#3863);
#2852=LINE('',#20782,#3864);
#2853=LINE('',#20783,#3865);
#2854=LINE('',#20785,#3866);
#2855=LINE('',#20789,#3867);
#2856=LINE('',#20791,#3868);
#2857=LINE('',#20792,#3869);
#2858=LINE('',#22254,#3870);
#2859=LINE('',#22256,#3871);
#2860=LINE('',#22258,#3872);
#2861=LINE('',#22259,#3873);
#2862=LINE('',#22263,#3874);
#2863=LINE('',#22265,#3875);
#2864=LINE('',#22267,#3876);
#2865=LINE('',#22269,#3877);
#2866=LINE('',#22271,#3878);
#2867=LINE('',#22272,#3879);
#2868=LINE('',#22276,#3880);
#2869=LINE('',#22278,#3881);
#2870=LINE('',#22280,#3882);
#2871=LINE('',#22285,#3883);
#2872=LINE('',#22289,#3884);
#2873=LINE('',#22290,#3885);
#2874=LINE('',#22294,#3886);
#2875=LINE('',#22296,#3887);
#2876=LINE('',#22298,#3888);
#2877=LINE('',#22299,#3889);
#2878=LINE('',#22303,#3890);
#2879=LINE('',#22306,#3891);
#2880=LINE('',#22310,#3892);
#2881=LINE('',#22313,#3893);
#2882=LINE('',#22317,#3894);
#2883=LINE('',#22319,#3895);
#2884=LINE('',#22321,#3896);
#2885=LINE('',#22322,#3897);
#2886=LINE('',#22326,#3898);
#2887=LINE('',#22329,#3899);
#2888=LINE('',#22333,#3900);
#2889=LINE('',#22336,#3901);
#2890=LINE('',#22340,#3902);
#2891=LINE('',#22342,#3903);
#2892=LINE('',#22344,#3904);
#2893=LINE('',#22345,#3905);
#2894=LINE('',#22349,#3906);
#2895=LINE('',#22351,#3907);
#2896=LINE('',#22354,#3908);
#2897=LINE('',#22358,#3909);
#2898=LINE('',#22362,#3910);
#2899=LINE('',#22363,#3911);
#2900=LINE('',#22367,#3912);
#2901=LINE('',#22369,#3913);
#2902=LINE('',#22371,#3914);
#2903=LINE('',#22372,#3915);
#2904=LINE('',#22376,#3916);
#2905=LINE('',#22378,#3917);
#2906=LINE('',#22381,#3918);
#2907=LINE('',#22384,#3919);
#2908=LINE('',#22388,#3920);
#2909=LINE('',#22390,#3921);
#2910=LINE('',#22392,#3922);
#2911=LINE('',#22393,#3923);
#2912=LINE('',#22396,#3924);
#2913=LINE('',#22399,#3925);
#2914=LINE('',#22403,#3926);
#2915=LINE('',#22405,#3927);
#2916=LINE('',#22409,#3928);
#2917=LINE('',#22411,#3929);
#2918=LINE('',#22413,#3930);
#2919=LINE('',#22414,#3931);
#2920=LINE('',#22418,#3932);
#2921=LINE('',#22420,#3933);
#2922=LINE('',#22422,#3934);
#2923=LINE('',#22423,#3935);
#2924=LINE('',#22427,#3936);
#2925=LINE('',#22429,#3937);
#2926=LINE('',#22431,#3938);
#2927=LINE('',#22432,#3939);
#2928=LINE('',#22436,#3940);
#2929=LINE('',#22438,#3941);
#2930=LINE('',#22440,#3942);
#2931=LINE('',#22441,#3943);
#2932=LINE('',#25208,#3944);
#2933=LINE('',#25218,#3945);
#2934=LINE('',#25226,#3946);
#2935=LINE('',#25233,#3947);
#2936=LINE('',#25236,#3948);
#2937=LINE('',#25241,#3949);
#2938=LINE('',#25287,#3950);
#2939=LINE('',#25291,#3951);
#2940=LINE('',#25295,#3952);
#2941=LINE('',#25300,#3953);
#2942=LINE('',#25306,#3954);
#2943=LINE('',#25309,#3955);
#2944=LINE('',#25312,#3956);
#2945=LINE('',#25316,#3957);
#2946=LINE('',#25320,#3958);
#2947=LINE('',#25324,#3959);
#2948=LINE('',#25328,#3960);
#2949=LINE('',#25332,#3961);
#2950=LINE('',#25336,#3962);
#2951=LINE('',#25340,#3963);
#2952=LINE('',#25346,#3964);
#2953=LINE('',#25349,#3965);
#2954=LINE('',#25352,#3966);
#2955=LINE('',#25356,#3967);
#2956=LINE('',#25360,#3968);
#2957=LINE('',#25364,#3969);
#2958=LINE('',#25368,#3970);
#2959=LINE('',#25372,#3971);
#2960=LINE('',#25375,#3972);
#2961=LINE('',#25378,#3973);
#2962=LINE('',#25382,#3974);
#2963=LINE('',#25384,#3975);
#2964=LINE('',#25385,#3976);
#2965=LINE('',#25388,#3977);
#2966=LINE('',#25390,#3978);
#2967=LINE('',#25391,#3979);
#2968=LINE('',#25394,#3980);
#2969=LINE('',#25396,#3981);
#2970=LINE('',#25397,#3982);
#2971=LINE('',#25400,#3983);
#2972=LINE('',#25402,#3984);
#2973=LINE('',#25403,#3985);
#2974=LINE('',#25406,#3986);
#2975=LINE('',#25408,#3987);
#2976=LINE('',#25409,#3988);
#2977=LINE('',#25412,#3989);
#2978=LINE('',#25414,#3990);
#2979=LINE('',#25415,#3991);
#2980=LINE('',#25418,#3992);
#2981=LINE('',#25420,#3993);
#2982=LINE('',#25421,#3994);
#2983=LINE('',#25424,#3995);
#2984=LINE('',#25426,#3996);
#2985=LINE('',#25427,#3997);
#2986=LINE('',#25430,#3998);
#2987=LINE('',#25432,#3999);
#2988=LINE('',#25433,#4000);
#2989=LINE('',#25436,#4001);
#2990=LINE('',#25438,#4002);
#2991=LINE('',#25439,#4003);
#2992=LINE('',#25442,#4004);
#2993=LINE('',#25446,#4005);
#2994=LINE('',#25448,#4006);
#2995=LINE('',#25449,#4007);
#2996=LINE('',#25451,#4008);
#2997=LINE('',#25455,#4009);
#2998=LINE('',#25457,#4010);
#2999=LINE('',#25458,#4011);
#3000=LINE('',#25460,#4012);
#3001=LINE('',#25464,#4013);
#3002=LINE('',#25466,#4014);
#3003=LINE('',#25467,#4015);
#3004=LINE('',#25469,#4016);
#3005=LINE('',#25473,#4017);
#3006=LINE('',#25475,#4018);
#3007=LINE('',#25476,#4019);
#3008=LINE('',#25478,#4020);
#3009=LINE('',#25482,#4021);
#3010=LINE('',#25484,#4022);
#3011=LINE('',#25485,#4023);
#3012=LINE('',#25487,#4024);
#3013=LINE('',#25491,#4025);
#3014=LINE('',#25493,#4026);
#3015=LINE('',#25494,#4027);
#3016=LINE('',#25496,#4028);
#3017=LINE('',#25500,#4029);
#3018=LINE('',#25502,#4030);
#3019=LINE('',#25503,#4031);
#3020=LINE('',#25505,#4032);
#3021=LINE('',#25509,#4033);
#3022=LINE('',#25511,#4034);
#3023=LINE('',#25512,#4035);
#3024=LINE('',#25514,#4036);
#3025=LINE('',#25518,#4037);
#3026=LINE('',#25520,#4038);
#3027=LINE('',#25521,#4039);
#3028=LINE('',#25523,#4040);
#3029=LINE('',#25527,#4041);
#3030=LINE('',#25529,#4042);
#3031=LINE('',#25530,#4043);
#3032=LINE('',#25532,#4044);
#3033=LINE('',#25534,#4045);
#3034=LINE('',#25535,#4046);
#3035=LINE('',#25538,#4047);
#3036=LINE('',#25540,#4048);
#3037=LINE('',#25541,#4049);
#3038=LINE('',#25546,#4050);
#3039=LINE('',#25548,#4051);
#3040=LINE('',#25549,#4052);
#3041=LINE('',#25553,#4053);
#3042=LINE('',#25554,#4054);
#3043=LINE('',#25557,#4055);
#3044=LINE('',#25560,#4056);
#3045=LINE('',#25563,#4057);
#3046=LINE('',#25567,#4058);
#3047=LINE('',#25569,#4059);
#3048=LINE('',#25570,#4060);
#3049=LINE('',#25574,#4061);
#3050=LINE('',#25575,#4062);
#3051=LINE('',#25578,#4063);
#3052=LINE('',#25581,#4064);
#3053=LINE('',#25584,#4065);
#3054=LINE('',#25587,#4066);
#3055=LINE('',#25589,#4067);
#3056=LINE('',#25590,#4068);
#3057=LINE('',#25594,#4069);
#3058=LINE('',#25595,#4070);
#3059=LINE('',#25598,#4071);
#3060=LINE('',#25601,#4072);
#3061=LINE('',#25604,#4073);
#3062=LINE('',#25607,#4074);
#3063=LINE('',#25609,#4075);
#3064=LINE('',#25610,#4076);
#3065=LINE('',#25614,#4077);
#3066=LINE('',#25615,#4078);
#3067=LINE('',#25618,#4079);
#3068=LINE('',#25621,#4080);
#3069=LINE('',#25624,#4081);
#3070=LINE('',#25627,#4082);
#3071=LINE('',#25629,#4083);
#3072=LINE('',#25630,#4084);
#3073=LINE('',#25634,#4085);
#3074=LINE('',#25635,#4086);
#3075=LINE('',#25638,#4087);
#3076=LINE('',#25641,#4088);
#3077=LINE('',#25644,#4089);
#3078=LINE('',#25647,#4090);
#3079=LINE('',#25649,#4091);
#3080=LINE('',#25650,#4092);
#3081=LINE('',#25654,#4093);
#3082=LINE('',#25655,#4094);
#3083=LINE('',#25658,#4095);
#3084=LINE('',#25661,#4096);
#3085=LINE('',#25664,#4097);
#3086=LINE('',#25667,#4098);
#3087=LINE('',#25669,#4099);
#3088=LINE('',#25670,#4100);
#3089=LINE('',#25674,#4101);
#3090=LINE('',#25675,#4102);
#3091=LINE('',#25678,#4103);
#3092=LINE('',#25681,#4104);
#3093=LINE('',#25684,#4105);
#3094=LINE('',#25687,#4106);
#3095=LINE('',#25689,#4107);
#3096=LINE('',#25690,#4108);
#3097=LINE('',#25694,#4109);
#3098=LINE('',#25695,#4110);
#3099=LINE('',#25698,#4111);
#3100=LINE('',#25701,#4112);
#3101=LINE('',#25704,#4113);
#3102=LINE('',#25707,#4114);
#3103=LINE('',#25709,#4115);
#3104=LINE('',#25710,#4116);
#3105=LINE('',#25714,#4117);
#3106=LINE('',#25715,#4118);
#3107=LINE('',#25718,#4119);
#3108=LINE('',#25721,#4120);
#3109=LINE('',#25724,#4121);
#3110=LINE('',#25727,#4122);
#3111=LINE('',#25729,#4123);
#3112=LINE('',#25730,#4124);
#3113=LINE('',#25734,#4125);
#3114=LINE('',#25735,#4126);
#3115=LINE('',#25738,#4127);
#3116=LINE('',#25741,#4128);
#3117=LINE('',#25744,#4129);
#3118=LINE('',#25766,#4130);
#3119=LINE('',#25768,#4131);
#3120=LINE('',#25791,#4132);
#3121=LINE('',#25796,#4133);
#3122=LINE('',#25801,#4134);
#3123=LINE('',#25806,#4135);
#3124=LINE('',#25811,#4136);
#3125=LINE('',#25816,#4137);
#3126=LINE('',#25821,#4138);
#3127=LINE('',#25826,#4139);
#3128=LINE('',#25831,#4140);
#3129=LINE('',#25836,#4141);
#3130=LINE('',#25841,#4142);
#3131=LINE('',#25846,#4143);
#3132=LINE('',#25851,#4144);
#3133=LINE('',#25854,#4145);
#3134=LINE('',#25861,#4146);
#3135=LINE('',#25863,#4147);
#3136=LINE('',#25865,#4148);
#3137=LINE('',#25866,#4149);
#3138=LINE('',#25869,#4150);
#3139=LINE('',#25871,#4151);
#3140=LINE('',#25872,#4152);
#3141=LINE('',#25877,#4153);
#3142=LINE('',#25881,#4154);
#3143=LINE('',#25883,#4155);
#3144=LINE('',#25884,#4156);
#3145=LINE('',#25889,#4157);
#3146=LINE('',#25893,#4158);
#3147=LINE('',#25895,#4159);
#3148=LINE('',#25896,#4160);
#3149=LINE('',#25901,#4161);
#3150=LINE('',#25905,#4162);
#3151=LINE('',#25907,#4163);
#3152=LINE('',#25908,#4164);
#3153=LINE('',#25913,#4165);
#3154=LINE('',#25917,#4166);
#3155=LINE('',#25919,#4167);
#3156=LINE('',#25920,#4168);
#3157=LINE('',#25923,#4169);
#3158=LINE('',#25925,#4170);
#3159=LINE('',#25926,#4171);
#3160=LINE('',#25928,#4172);
#3161=LINE('',#25929,#4173);
#3162=LINE('',#25935,#4174);
#3163=LINE('',#25939,#4175);
#3164=LINE('',#25943,#4176);
#3165=LINE('',#25947,#4177);
#3166=LINE('',#25951,#4178);
#3167=LINE('',#25953,#4179);
#3168=LINE('',#25955,#4180);
#3169=LINE('',#25956,#4181);
#3170=LINE('',#25959,#4182);
#3171=LINE('',#25961,#4183);
#3172=LINE('',#25962,#4184);
#3173=LINE('',#25965,#4185);
#3174=LINE('',#25966,#4186);
#3175=LINE('',#25969,#4187);
#3176=LINE('',#25970,#4188);
#3177=LINE('',#25973,#4189);
#3178=LINE('',#25977,#4190);
#3179=LINE('',#25978,#4191);
#3180=LINE('',#25981,#4192);
#3181=LINE('',#25985,#4193);
#3182=LINE('',#25986,#4194);
#3183=LINE('',#25989,#4195);
#3184=LINE('',#25993,#4196);
#3185=LINE('',#25994,#4197);
#3186=LINE('',#25997,#4198);
#3187=LINE('',#26001,#4199);
#3188=LINE('',#26002,#4200);
#3189=LINE('',#26004,#4201);
#3190=LINE('',#26009,#4202);
#3191=LINE('',#26011,#4203);
#3192=LINE('',#26013,#4204);
#3193=LINE('',#26015,#4205);
#3194=LINE('',#26017,#4206);
#3195=LINE('',#26021,#4207);
#3196=LINE('',#26025,#4208);
#3197=LINE('',#26029,#4209);
#3198=LINE('',#26033,#4210);
#3199=LINE('',#26035,#4211);
#3200=LINE('',#26036,#4212);
#3201=LINE('',#26039,#4213);
#3202=LINE('',#26040,#4214);
#3203=LINE('',#26043,#4215);
#3204=LINE('',#26044,#4216);
#3205=LINE('',#26048,#4217);
#3206=LINE('',#26051,#4218);
#3207=LINE('',#26052,#4219);
#3208=LINE('',#26056,#4220);
#3209=LINE('',#26059,#4221);
#3210=LINE('',#26060,#4222);
#3211=LINE('',#26064,#4223);
#3212=LINE('',#26067,#4224);
#3213=LINE('',#26068,#4225);
#3214=LINE('',#26072,#4226);
#3215=LINE('',#26075,#4227);
#3216=LINE('',#26076,#4228);
#3217=LINE('',#26078,#4229);
#3218=LINE('',#26083,#4230);
#3219=LINE('',#26085,#4231);
#3220=LINE('',#26087,#4232);
#3221=LINE('',#26088,#4233);
#3222=LINE('',#26091,#4234);
#3223=LINE('',#26093,#4235);
#3224=LINE('',#26094,#4236);
#3225=LINE('',#26100,#4237);
#3226=LINE('',#26103,#4238);
#3227=LINE('',#26105,#4239);
#3228=LINE('',#26106,#4240);
#3229=LINE('',#26112,#4241);
#3230=LINE('',#26115,#4242);
#3231=LINE('',#26117,#4243);
#3232=LINE('',#26118,#4244);
#3233=LINE('',#26124,#4245);
#3234=LINE('',#26127,#4246);
#3235=LINE('',#26129,#4247);
#3236=LINE('',#26130,#4248);
#3237=LINE('',#26136,#4249);
#3238=LINE('',#26139,#4250);
#3239=LINE('',#26141,#4251);
#3240=LINE('',#26142,#4252);
#3241=LINE('',#26145,#4253);
#3242=LINE('',#26147,#4254);
#3243=LINE('',#26148,#4255);
#3244=LINE('',#26150,#4256);
#3245=LINE('',#26151,#4257);
#3246=LINE('',#26157,#4258);
#3247=LINE('',#26159,#4259);
#3248=LINE('',#26161,#4260);
#3249=LINE('',#26162,#4261);
#3250=LINE('',#26165,#4262);
#3251=LINE('',#26167,#4263);
#3252=LINE('',#26168,#4264);
#3253=LINE('',#26173,#4265);
#3254=LINE('',#26177,#4266);
#3255=LINE('',#26179,#4267);
#3256=LINE('',#26180,#4268);
#3257=LINE('',#26185,#4269);
#3258=LINE('',#26189,#4270);
#3259=LINE('',#26191,#4271);
#3260=LINE('',#26192,#4272);
#3261=LINE('',#26197,#4273);
#3262=LINE('',#26201,#4274);
#3263=LINE('',#26203,#4275);
#3264=LINE('',#26204,#4276);
#3265=LINE('',#26209,#4277);
#3266=LINE('',#26213,#4278);
#3267=LINE('',#26215,#4279);
#3268=LINE('',#26216,#4280);
#3269=LINE('',#26219,#4281);
#3270=LINE('',#26221,#4282);
#3271=LINE('',#26222,#4283);
#3272=LINE('',#26224,#4284);
#3273=LINE('',#26225,#4285);
#3274=LINE('',#26231,#4286);
#3275=LINE('',#26233,#4287);
#3276=LINE('',#26235,#4288);
#3277=LINE('',#26237,#4289);
#3278=LINE('',#26239,#4290);
#3279=LINE('',#26243,#4291);
#3280=LINE('',#26247,#4292);
#3281=LINE('',#26251,#4293);
#3282=LINE('',#26255,#4294);
#3283=LINE('',#26257,#4295);
#3284=LINE('',#26258,#4296);
#3285=LINE('',#26261,#4297);
#3286=LINE('',#26262,#4298);
#3287=LINE('',#26265,#4299);
#3288=LINE('',#26266,#4300);
#3289=LINE('',#26270,#4301);
#3290=LINE('',#26273,#4302);
#3291=LINE('',#26274,#4303);
#3292=LINE('',#26278,#4304);
#3293=LINE('',#26281,#4305);
#3294=LINE('',#26282,#4306);
#3295=LINE('',#26286,#4307);
#3296=LINE('',#26289,#4308);
#3297=LINE('',#26290,#4309);
#3298=LINE('',#26294,#4310);
#3299=LINE('',#26297,#4311);
#3300=LINE('',#26298,#4312);
#3301=LINE('',#26300,#4313);
#3302=LINE('',#26305,#4314);
#3303=LINE('',#26307,#4315);
#3304=LINE('',#26309,#4316);
#3305=LINE('',#26310,#4317);
#3306=LINE('',#26313,#4318);
#3307=LINE('',#26315,#4319);
#3308=LINE('',#26316,#4320);
#3309=LINE('',#26321,#4321);
#3310=LINE('',#26325,#4322);
#3311=LINE('',#26327,#4323);
#3312=LINE('',#26328,#4324);
#3313=LINE('',#26333,#4325);
#3314=LINE('',#26337,#4326);
#3315=LINE('',#26339,#4327);
#3316=LINE('',#26340,#4328);
#3317=LINE('',#26345,#4329);
#3318=LINE('',#26349,#4330);
#3319=LINE('',#26351,#4331);
#3320=LINE('',#26352,#4332);
#3321=LINE('',#26357,#4333);
#3322=LINE('',#26361,#4334);
#3323=LINE('',#26363,#4335);
#3324=LINE('',#26364,#4336);
#3325=LINE('',#26367,#4337);
#3326=LINE('',#26369,#4338);
#3327=LINE('',#26370,#4339);
#3328=LINE('',#26372,#4340);
#3329=LINE('',#26373,#4341);
#3330=LINE('',#26379,#4342);
#3331=LINE('',#26381,#4343);
#3332=LINE('',#26383,#4344);
#3333=LINE('',#26385,#4345);
#3334=LINE('',#26387,#4346);
#3335=LINE('',#26391,#4347);
#3336=LINE('',#26395,#4348);
#3337=LINE('',#26399,#4349);
#3338=LINE('',#26403,#4350);
#3339=LINE('',#26405,#4351);
#3340=LINE('',#26406,#4352);
#3341=LINE('',#26409,#4353);
#3342=LINE('',#26410,#4354);
#3343=LINE('',#26413,#4355);
#3344=LINE('',#26414,#4356);
#3345=LINE('',#26418,#4357);
#3346=LINE('',#26421,#4358);
#3347=LINE('',#26422,#4359);
#3348=LINE('',#26426,#4360);
#3349=LINE('',#26429,#4361);
#3350=LINE('',#26430,#4362);
#3351=LINE('',#26434,#4363);
#3352=LINE('',#26437,#4364);
#3353=LINE('',#26438,#4365);
#3354=LINE('',#26442,#4366);
#3355=LINE('',#26445,#4367);
#3356=LINE('',#26446,#4368);
#3357=LINE('',#26448,#4369);
#3358=LINE('',#26453,#4370);
#3359=LINE('',#26455,#4371);
#3360=LINE('',#26459,#4372);
#3361=LINE('',#26463,#4373);
#3362=LINE('',#26467,#4374);
#3363=LINE('',#26471,#4375);
#3364=LINE('',#26473,#4376);
#3365=LINE('',#26474,#4377);
#3366=LINE('',#26477,#4378);
#3367=LINE('',#26479,#4379);
#3368=LINE('',#26480,#4380);
#3369=LINE('',#26483,#4381);
#3370=LINE('',#26484,#4382);
#3371=LINE('',#26487,#4383);
#3372=LINE('',#26488,#4384);
#3373=LINE('',#26491,#4385);
#3374=LINE('',#26495,#4386);
#3375=LINE('',#26496,#4387);
#3376=LINE('',#26499,#4388);
#3377=LINE('',#26503,#4389);
#3378=LINE('',#26504,#4390);
#3379=LINE('',#26507,#4391);
#3380=LINE('',#26511,#4392);
#3381=LINE('',#26512,#4393);
#3382=LINE('',#26515,#4394);
#3383=LINE('',#26519,#4395);
#3384=LINE('',#26520,#4396);
#3385=LINE('',#26522,#4397);
#3386=LINE('',#26527,#4398);
#3387=LINE('',#26529,#4399);
#3388=LINE('',#26531,#4400);
#3389=LINE('',#26533,#4401);
#3390=LINE('',#26537,#4402);
#3391=LINE('',#26541,#4403);
#3392=LINE('',#26545,#4404);
#3393=LINE('',#26548,#4405);
#3394=LINE('',#26551,#4406);
#3395=LINE('',#26553,#4407);
#3396=LINE('',#26554,#4408);
#3397=LINE('',#26557,#4409);
#3398=LINE('',#26558,#4410);
#3399=LINE('',#26561,#4411);
#3400=LINE('',#26562,#4412);
#3401=LINE('',#26566,#4413);
#3402=LINE('',#26569,#4414);
#3403=LINE('',#26570,#4415);
#3404=LINE('',#26574,#4416);
#3405=LINE('',#26577,#4417);
#3406=LINE('',#26578,#4418);
#3407=LINE('',#26582,#4419);
#3408=LINE('',#26585,#4420);
#3409=LINE('',#26586,#4421);
#3410=LINE('',#26590,#4422);
#3411=LINE('',#26593,#4423);
#3412=LINE('',#26594,#4424);
#3413=LINE('',#26596,#4425);
#3414=LINE('',#26601,#4426);
#3415=LINE('',#26603,#4427);
#3416=LINE('',#26605,#4428);
#3417=LINE('',#26606,#4429);
#3418=LINE('',#26609,#4430);
#3419=LINE('',#26611,#4431);
#3420=LINE('',#26612,#4432);
#3421=LINE('',#26617,#4433);
#3422=LINE('',#26621,#4434);
#3423=LINE('',#26623,#4435);
#3424=LINE('',#26624,#4436);
#3425=LINE('',#26629,#4437);
#3426=LINE('',#26633,#4438);
#3427=LINE('',#26635,#4439);
#3428=LINE('',#26636,#4440);
#3429=LINE('',#26641,#4441);
#3430=LINE('',#26645,#4442);
#3431=LINE('',#26647,#4443);
#3432=LINE('',#26648,#4444);
#3433=LINE('',#26650,#4445);
#3434=LINE('',#26651,#4446);
#3435=LINE('',#26657,#4447);
#3436=LINE('',#26659,#4448);
#3437=LINE('',#26661,#4449);
#3438=LINE('',#26662,#4450);
#3439=LINE('',#26665,#4451);
#3440=LINE('',#26667,#4452);
#3441=LINE('',#26668,#4453);
#3442=LINE('',#26673,#4454);
#3443=LINE('',#26677,#4455);
#3444=LINE('',#26679,#4456);
#3445=LINE('',#26680,#4457);
#3446=LINE('',#26685,#4458);
#3447=LINE('',#26689,#4459);
#3448=LINE('',#26691,#4460);
#3449=LINE('',#26692,#4461);
#3450=LINE('',#26697,#4462);
#3451=LINE('',#26701,#4463);
#3452=LINE('',#26703,#4464);
#3453=LINE('',#26704,#4465);
#3454=LINE('',#26706,#4466);
#3455=LINE('',#26707,#4467);
#3456=LINE('',#26713,#4468);
#3457=LINE('',#26715,#4469);
#3458=LINE('',#26717,#4470);
#3459=LINE('',#26718,#4471);
#3460=LINE('',#26721,#4472);
#3461=LINE('',#26723,#4473);
#3462=LINE('',#26724,#4474);
#3463=LINE('',#26730,#4475);
#3464=LINE('',#26733,#4476);
#3465=LINE('',#26735,#4477);
#3466=LINE('',#26736,#4478);
#3467=LINE('',#26742,#4479);
#3468=LINE('',#26745,#4480);
#3469=LINE('',#26747,#4481);
#3470=LINE('',#26748,#4482);
#3471=LINE('',#26754,#4483);
#3472=LINE('',#26757,#4484);
#3473=LINE('',#26759,#4485);
#3474=LINE('',#26760,#4486);
#3475=LINE('',#26762,#4487);
#3476=LINE('',#26763,#4488);
#3477=LINE('',#26769,#4489);
#3478=LINE('',#26771,#4490);
#3479=LINE('',#26773,#4491);
#3480=LINE('',#26774,#4492);
#3481=LINE('',#26777,#4493);
#3482=LINE('',#26779,#4494);
#3483=LINE('',#26780,#4495);
#3484=LINE('',#26786,#4496);
#3485=LINE('',#26789,#4497);
#3486=LINE('',#26791,#4498);
#3487=LINE('',#26792,#4499);
#3488=LINE('',#26798,#4500);
#3489=LINE('',#26801,#4501);
#3490=LINE('',#26803,#4502);
#3491=LINE('',#26804,#4503);
#3492=LINE('',#26810,#4504);
#3493=LINE('',#26813,#4505);
#3494=LINE('',#26815,#4506);
#3495=LINE('',#26816,#4507);
#3496=LINE('',#26818,#4508);
#3497=LINE('',#26819,#4509);
#3498=LINE('',#26825,#4510);
#3499=LINE('',#26827,#4511);
#3500=LINE('',#26831,#4512);
#3501=LINE('',#26835,#4513);
#3502=LINE('',#26839,#4514);
#3503=LINE('',#26840,#4515);
#3504=LINE('',#26843,#4516);
#3505=LINE('',#26845,#4517);
#3506=LINE('',#26846,#4518);
#3507=LINE('',#26849,#4519);
#3508=LINE('',#26850,#4520);
#3509=LINE('',#26853,#4521);
#3510=LINE('',#26857,#4522);
#3511=LINE('',#26858,#4523);
#3512=LINE('',#26861,#4524);
#3513=LINE('',#26865,#4525);
#3514=LINE('',#26866,#4526);
#3515=LINE('',#26869,#4527);
#3516=LINE('',#26873,#4528);
#3517=LINE('',#26874,#4529);
#3518=LINE('',#26876,#4530);
#3519=LINE('',#26881,#4531);
#3520=LINE('',#26883,#4532);
#3521=LINE('',#26885,#4533);
#3522=LINE('',#26886,#4534);
#3523=LINE('',#26889,#4535);
#3524=LINE('',#26891,#4536);
#3525=LINE('',#26892,#4537);
#3526=LINE('',#26897,#4538);
#3527=LINE('',#26901,#4539);
#3528=LINE('',#26903,#4540);
#3529=LINE('',#26904,#4541);
#3530=LINE('',#26909,#4542);
#3531=LINE('',#26913,#4543);
#3532=LINE('',#26915,#4544);
#3533=LINE('',#26916,#4545);
#3534=LINE('',#26921,#4546);
#3535=LINE('',#26925,#4547);
#3536=LINE('',#26927,#4548);
#3537=LINE('',#26928,#4549);
#3538=LINE('',#26930,#4550);
#3539=LINE('',#26931,#4551);
#3540=LINE('',#26937,#4552);
#3541=LINE('',#26939,#4553);
#3542=LINE('',#26941,#4554);
#3543=LINE('',#26945,#4555);
#3544=LINE('',#26949,#4556);
#3545=LINE('',#26952,#4557);
#3546=LINE('',#26955,#4558);
#3547=LINE('',#26957,#4559);
#3548=LINE('',#26958,#4560);
#3549=LINE('',#26961,#4561);
#3550=LINE('',#26962,#4562);
#3551=LINE('',#26966,#4563);
#3552=LINE('',#26969,#4564);
#3553=LINE('',#26970,#4565);
#3554=LINE('',#26974,#4566);
#3555=LINE('',#26977,#4567);
#3556=LINE('',#26978,#4568);
#3557=LINE('',#26982,#4569);
#3558=LINE('',#26985,#4570);
#3559=LINE('',#26986,#4571);
#3560=LINE('',#26988,#4572);
#3561=LINE('',#26993,#4573);
#3562=LINE('',#26995,#4574);
#3563=LINE('',#26997,#4575);
#3564=LINE('',#27001,#4576);
#3565=LINE('',#27005,#4577);
#3566=LINE('',#27008,#4578);
#3567=LINE('',#27011,#4579);
#3568=LINE('',#27013,#4580);
#3569=LINE('',#27014,#4581);
#3570=LINE('',#27017,#4582);
#3571=LINE('',#27018,#4583);
#3572=LINE('',#27022,#4584);
#3573=LINE('',#27025,#4585);
#3574=LINE('',#27026,#4586);
#3575=LINE('',#27030,#4587);
#3576=LINE('',#27033,#4588);
#3577=LINE('',#27034,#4589);
#3578=LINE('',#27038,#4590);
#3579=LINE('',#27041,#4591);
#3580=LINE('',#27042,#4592);
#3581=LINE('',#27044,#4593);
#3582=LINE('',#27049,#4594);
#3583=LINE('',#27051,#4595);
#3584=LINE('',#27053,#4596);
#3585=LINE('',#27054,#4597);
#3586=LINE('',#27057,#4598);
#3587=LINE('',#27059,#4599);
#3588=LINE('',#27060,#4600);
#3589=LINE('',#27066,#4601);
#3590=LINE('',#27069,#4602);
#3591=LINE('',#27071,#4603);
#3592=LINE('',#27072,#4604);
#3593=LINE('',#27078,#4605);
#3594=LINE('',#27081,#4606);
#3595=LINE('',#27083,#4607);
#3596=LINE('',#27084,#4608);
#3597=LINE('',#27090,#4609);
#3598=LINE('',#27093,#4610);
#3599=LINE('',#27095,#4611);
#3600=LINE('',#27096,#4612);
#3601=LINE('',#27098,#4613);
#3602=LINE('',#27099,#4614);
#3603=LINE('',#27105,#4615);
#3604=LINE('',#27107,#4616);
#3605=LINE('',#27111,#4617);
#3606=LINE('',#27115,#4618);
#3607=LINE('',#27119,#4619);
#3608=LINE('',#27120,#4620);
#3609=LINE('',#27123,#4621);
#3610=LINE('',#27125,#4622);
#3611=LINE('',#27126,#4623);
#3612=LINE('',#27129,#4624);
#3613=LINE('',#27130,#4625);
#3614=LINE('',#27133,#4626);
#3615=LINE('',#27137,#4627);
#3616=LINE('',#27138,#4628);
#3617=LINE('',#27141,#4629);
#3618=LINE('',#27145,#4630);
#3619=LINE('',#27146,#4631);
#3620=LINE('',#27149,#4632);
#3621=LINE('',#27153,#4633);
#3622=LINE('',#27154,#4634);
#3623=LINE('',#27156,#4635);
#3624=LINE('',#27163,#4636);
#3625=LINE('',#27166,#4637);
#3626=LINE('',#27172,#4638);
#3627=LINE('',#27175,#4639);
#3628=LINE('',#27181,#4640);
#3629=LINE('',#27184,#4641);
#3630=LINE('',#27190,#4642);
#3631=LINE('',#27193,#4643);
#3632=LINE('',#27197,#4644);
#3633=LINE('',#27199,#4645);
#3634=LINE('',#27201,#4646);
#3635=LINE('',#27202,#4647);
#3636=LINE('',#27206,#4648);
#3637=LINE('',#27208,#4649);
#3638=LINE('',#27210,#4650);
#3639=LINE('',#27211,#4651);
#3640=LINE('',#27215,#4652);
#3641=LINE('',#27217,#4653);
#3642=LINE('',#27219,#4654);
#3643=LINE('',#27220,#4655);
#3644=LINE('',#27224,#4656);
#3645=LINE('',#27226,#4657);
#3646=LINE('',#27228,#4658);
#3647=LINE('',#27229,#4659);
#3648=LINE('',#27231,#4660);
#3649=LINE('',#27232,#4661);
#3650=LINE('',#27233,#4662);
#3651=LINE('',#27234,#4663);
#3652=LINE('',#27236,#4664);
#3653=LINE('',#27238,#4665);
#3654=LINE('',#27241,#4666);
#3655=LINE('',#27243,#4667);
#3656=LINE('',#27246,#4668);
#3657=LINE('',#27248,#4669);
#3658=LINE('',#27251,#4670);
#3659=LINE('',#27253,#4671);
#3660=LINE('',#27256,#4672);
#3661=LINE('',#27257,#4673);
#3662=LINE('',#27258,#4674);
#3663=LINE('',#27259,#4675);
#3664=LINE('',#27261,#4676);
#3665=LINE('',#27264,#4677);
#3666=LINE('',#27266,#4678);
#3667=LINE('',#27269,#4679);
#3668=LINE('',#27271,#4680);
#3669=LINE('',#27274,#4681);
#3670=LINE('',#27276,#4682);
#3671=LINE('',#27279,#4683);
#3672=LINE('',#27281,#4684);
#3673=LINE('',#27283,#4685);
#3674=LINE('',#27286,#4686);
#3675=LINE('',#27288,#4687);
#3676=LINE('',#27291,#4688);
#3677=LINE('',#27293,#4689);
#3678=LINE('',#27296,#4690);
#3679=LINE('',#27298,#4691);
#3680=LINE('',#27308,#4692);
#3681=LINE('',#27314,#4693);
#3682=LINE('',#27319,#4694);
#3683=LINE('',#27321,#4695);
#3684=LINE('',#27323,#4696);
#3685=LINE('',#27324,#4697);
#3686=LINE('',#27327,#4698);
#3687=LINE('',#27329,#4699);
#3688=LINE('',#27330,#4700);
#3689=LINE('',#27335,#4701);
#3690=LINE('',#27339,#4702);
#3691=LINE('',#27341,#4703);
#3692=LINE('',#27342,#4704);
#3693=LINE('',#27347,#4705);
#3694=LINE('',#27351,#4706);
#3695=LINE('',#27353,#4707);
#3696=LINE('',#27354,#4708);
#3697=LINE('',#27359,#4709);
#3698=LINE('',#27363,#4710);
#3699=LINE('',#27365,#4711);
#3700=LINE('',#27366,#4712);
#3701=LINE('',#27371,#4713);
#3702=LINE('',#27375,#4714);
#3703=LINE('',#27377,#4715);
#3704=LINE('',#27378,#4716);
#3705=LINE('',#27381,#4717);
#3706=LINE('',#27383,#4718);
#3707=LINE('',#27384,#4719);
#3708=LINE('',#27386,#4720);
#3709=LINE('',#27387,#4721);
#3710=LINE('',#27394,#4722);
#3711=LINE('',#27400,#4723);
#3712=LINE('',#27405,#4724);
#3713=LINE('',#27407,#4725);
#3714=LINE('',#27409,#4726);
#3715=LINE('',#27410,#4727);
#3716=LINE('',#27413,#4728);
#3717=LINE('',#27415,#4729);
#3718=LINE('',#27416,#4730);
#3719=LINE('',#27421,#4731);
#3720=LINE('',#27425,#4732);
#3721=LINE('',#27427,#4733);
#3722=LINE('',#27428,#4734);
#3723=LINE('',#27433,#4735);
#3724=LINE('',#27437,#4736);
#3725=LINE('',#27439,#4737);
#3726=LINE('',#27440,#4738);
#3727=LINE('',#27445,#4739);
#3728=LINE('',#27449,#4740);
#3729=LINE('',#27451,#4741);
#3730=LINE('',#27452,#4742);
#3731=LINE('',#27454,#4743);
#3732=LINE('',#27455,#4744);
#3733=LINE('',#27462,#4745);
#3734=LINE('',#27468,#4746);
#3735=LINE('',#27473,#4747);
#3736=LINE('',#27475,#4748);
#3737=LINE('',#27477,#4749);
#3738=LINE('',#27478,#4750);
#3739=LINE('',#27481,#4751);
#3740=LINE('',#27483,#4752);
#3741=LINE('',#27484,#4753);
#3742=LINE('',#27490,#4754);
#3743=LINE('',#27493,#4755);
#3744=LINE('',#27495,#4756);
#3745=LINE('',#27496,#4757);
#3746=LINE('',#27502,#4758);
#3747=LINE('',#27505,#4759);
#3748=LINE('',#27507,#4760);
#3749=LINE('',#27508,#4761);
#3750=LINE('',#27514,#4762);
#3751=LINE('',#27517,#4763);
#3752=LINE('',#27519,#4764);
#3753=LINE('',#27520,#4765);
#3754=LINE('',#27522,#4766);
#3755=LINE('',#27523,#4767);
#3756=VECTOR('',#13183,160.);
#3757=VECTOR('',#13200,1000.);
#3758=VECTOR('',#13203,1000.);
#3759=VECTOR('',#13210,1000.);
#3760=VECTOR('',#13213,1000.);
#3761=VECTOR('',#13218,1000.);
#3762=VECTOR('',#13221,1000.);
#3763=VECTOR('',#13278,5.025);
#3764=VECTOR('',#13285,4.49999999999998);
#3765=VECTOR('',#13290,5.025);
#3766=VECTOR('',#13297,4.49999999999998);
#3767=VECTOR('',#13302,5.025);
#3768=VECTOR('',#13309,4.49999999999998);
#3769=VECTOR('',#13314,5.025);
#3770=VECTOR('',#13321,4.49999999999998);
#3771=VECTOR('',#13326,5.025);
#3772=VECTOR('',#13333,4.49999999999998);
#3773=VECTOR('',#13338,5.025);
#3774=VECTOR('',#13345,4.49999999999998);
#3775=VECTOR('',#13348,195.);
#3776=VECTOR('',#13353,35.5);
#3777=VECTOR('',#13362,35.5);
#3778=VECTOR('',#13367,35.5);
#3779=VECTOR('',#13372,4.5);
#3780=VECTOR('',#13379,4.5);
#3781=VECTOR('',#13386,4.5);
#3782=VECTOR('',#13393,4.5);
#3783=VECTOR('',#13400,1000.);
#3784=VECTOR('',#13403,1000.);
#3785=VECTOR('',#13410,160.);
#3786=VECTOR('',#13413,1000.);
#3787=VECTOR('',#13420,1000.);
#3788=VECTOR('',#13425,1000.);
#3789=VECTOR('',#13428,170.);
#3790=VECTOR('',#13429,1000.);
#3791=VECTOR('',#13430,170.);
#3792=VECTOR('',#13439,1000.);
#3793=VECTOR('',#13444,1000.);
#3794=VECTOR('',#13449,1000.);
#3795=VECTOR('',#13454,1000.);
#3796=VECTOR('',#13457,1000.);
#3797=VECTOR('',#13460,1000.);
#3798=VECTOR('',#13463,1000.);
#3799=VECTOR('',#13466,1000.);
#3800=VECTOR('',#13469,1000.);
#3801=VECTOR('',#13472,1000.);
#3802=VECTOR('',#13473,1000.);
#3803=VECTOR('',#13474,1000.);
#3804=VECTOR('',#13475,1000.);
#3805=VECTOR('',#13476,1000.);
#3806=VECTOR('',#13477,1000.);
#3807=VECTOR('',#13480,1000.);
#3808=VECTOR('',#13481,1000.);
#3809=VECTOR('',#13482,1000.);
#3810=VECTOR('',#13483,1000.);
#3811=VECTOR('',#13484,1000.);
#3812=VECTOR('',#13485,1000.);
#3813=VECTOR('',#13488,1000.);
#3814=VECTOR('',#13491,1000.);
#3815=VECTOR('',#13492,1000.);
#3816=VECTOR('',#13493,1000.);
#3817=VECTOR('',#13496,1000.);
#3818=VECTOR('',#13499,1000.);
#3819=VECTOR('',#13500,1000.);
#3820=VECTOR('',#13501,1000.);
#3821=VECTOR('',#13504,1000.);
#3822=VECTOR('',#13505,1000.);
#3823=VECTOR('',#13506,1000.);
#3824=VECTOR('',#13507,1000.);
#3825=VECTOR('',#13508,1000.);
#3826=VECTOR('',#13509,1000.);
#3827=VECTOR('',#13510,1000.);
#3828=VECTOR('',#13513,1000.);
#3829=VECTOR('',#13516,1000.);
#3830=VECTOR('',#13517,1000.);
#3831=VECTOR('',#13520,1000.);
#3832=VECTOR('',#13531,1000.);
#3833=VECTOR('',#13540,1000.);
#3834=VECTOR('',#13549,1000.);
#3835=VECTOR('',#13564,1000.);
#3836=VECTOR('',#13567,1000.);
#3837=VECTOR('',#13570,1000.);
#3838=VECTOR('',#13573,1000.);
#3839=VECTOR('',#13576,1000.);
#3840=VECTOR('',#13579,1000.);
#3841=VECTOR('',#13582,1000.);
#3842=VECTOR('',#13585,1000.);
#3843=VECTOR('',#13588,1000.);
#3844=VECTOR('',#13595,1000.);
#3845=VECTOR('',#13596,1000.);
#3846=VECTOR('',#13601,1000.);
#3847=VECTOR('',#13604,1000.);
#3848=VECTOR('',#13605,1000.);
#3849=VECTOR('',#13608,1000.);
#3850=VECTOR('',#13611,1000.);
#3851=VECTOR('',#13612,1000.);
#3852=VECTOR('',#13615,1000.);
#3853=VECTOR('',#13616,1000.);
#3854=VECTOR('',#13617,1000.);
#3855=VECTOR('',#13712,1000.);
#3856=VECTOR('',#13721,1000.);
#3857=VECTOR('',#13732,1000.);
#3858=VECTOR('',#13741,1000.);
#3859=VECTOR('',#13752,1000.);
#3860=VECTOR('',#13753,1000.);
#3861=VECTOR('',#13758,1000.);
#3862=VECTOR('',#13759,1000.);
#3863=VECTOR('',#13760,1000.);
#3864=VECTOR('',#13765,1000.);
#3865=VECTOR('',#13766,1000.);
#3866=VECTOR('',#13767,1000.);
#3867=VECTOR('',#13772,1000.);
#3868=VECTOR('',#13773,1000.);
#3869=VECTOR('',#13774,1000.);
#3870=VECTOR('',#13863,1000.);
#3871=VECTOR('',#13864,1000.);
#3872=VECTOR('',#13865,1000.);
#3873=VECTOR('',#13866,1000.);
#3874=VECTOR('',#13869,1000.);
#3875=VECTOR('',#13870,1000.);
#3876=VECTOR('',#13871,1000.);
#3877=VECTOR('',#13872,1000.);
#3878=VECTOR('',#13873,1000.);
#3879=VECTOR('',#13874,1000.);
#3880=VECTOR('',#13877,1000.);
#3881=VECTOR('',#13878,1000.);
#3882=VECTOR('',#13879,1000.);
#3883=VECTOR('',#13884,1000.);
#3884=VECTOR('',#13887,1000.);
#3885=VECTOR('',#13888,1000.);
#3886=VECTOR('',#13891,1000.);
#3887=VECTOR('',#13892,1000.);
#3888=VECTOR('',#13893,1000.);
#3889=VECTOR('',#13894,1000.);
#3890=VECTOR('',#13897,1000.);
#3891=VECTOR('',#13900,1000.);
#3892=VECTOR('',#13903,1000.);
#3893=VECTOR('',#13906,1000.);
#3894=VECTOR('',#13909,1000.);
#3895=VECTOR('',#13910,1000.);
#3896=VECTOR('',#13911,1000.);
#3897=VECTOR('',#13912,1000.);
#3898=VECTOR('',#13915,1000.);
#3899=VECTOR('',#13918,1000.);
#3900=VECTOR('',#13921,1000.);
#3901=VECTOR('',#13924,1000.);
#3902=VECTOR('',#13927,1000.);
#3903=VECTOR('',#13928,1000.);
#3904=VECTOR('',#13929,1000.);
#3905=VECTOR('',#13930,1000.);
#3906=VECTOR('',#13933,1000.);
#3907=VECTOR('',#13934,1000.);
#3908=VECTOR('',#13937,1000.);
#3909=VECTOR('',#13940,1000.);
#3910=VECTOR('',#13943,1000.);
#3911=VECTOR('',#13944,1000.);
#3912=VECTOR('',#13947,1000.);
#3913=VECTOR('',#13948,1000.);
#3914=VECTOR('',#13949,1000.);
#3915=VECTOR('',#13950,1000.);
#3916=VECTOR('',#13953,1000.);
#3917=VECTOR('',#13956,1000.);
#3918=VECTOR('',#13959,1000.);
#3919=VECTOR('',#13962,1000.);
#3920=VECTOR('',#13965,1000.);
#3921=VECTOR('',#13966,1000.);
#3922=VECTOR('',#13967,1000.);
#3923=VECTOR('',#13968,1000.);
#3924=VECTOR('',#13971,1000.);
#3925=VECTOR('',#13974,1000.);
#3926=VECTOR('',#13977,1000.);
#3927=VECTOR('',#13980,1000.);
#3928=VECTOR('',#13983,1000.);
#3929=VECTOR('',#13984,1000.);
#3930=VECTOR('',#13985,1000.);
#3931=VECTOR('',#13986,1000.);
#3932=VECTOR('',#13989,1000.);
#3933=VECTOR('',#13990,1000.);
#3934=VECTOR('',#13991,1000.);
#3935=VECTOR('',#13992,1000.);
#3936=VECTOR('',#13995,1000.);
#3937=VECTOR('',#13996,1000.);
#3938=VECTOR('',#13997,1000.);
#3939=VECTOR('',#13998,1000.);
#3940=VECTOR('',#14001,1000.);
#3941=VECTOR('',#14002,1000.);
#3942=VECTOR('',#14003,1000.);
#3943=VECTOR('',#14004,1000.);
#3944=VECTOR('',#14429,37.0000000000001);
#3945=VECTOR('',#14440,30.);
#3946=VECTOR('',#14449,35.);
#3947=VECTOR('',#14456,1000.);
#3948=VECTOR('',#14459,1000.);
#3949=VECTOR('',#14464,120.);
#3950=VECTOR('',#14511,160.);
#3951=VECTOR('',#14514,1000.);
#3952=VECTOR('',#14517,160.);
#3953=VECTOR('',#14522,1000.);
#3954=VECTOR('',#14527,1000.);
#3955=VECTOR('',#14530,1000.);
#3956=VECTOR('',#14531,1000.);
#3957=VECTOR('',#14534,1000.);
#3958=VECTOR('',#14537,1000.);
#3959=VECTOR('',#14540,1000.);
#3960=VECTOR('',#14543,1000.);
#3961=VECTOR('',#14546,1000.);
#3962=VECTOR('',#14549,1000.);
#3963=VECTOR('',#14552,1000.);
#3964=VECTOR('',#14557,1000.);
#3965=VECTOR('',#14560,1000.);
#3966=VECTOR('',#14561,1000.);
#3967=VECTOR('',#14564,1000.);
#3968=VECTOR('',#14567,1000.);
#3969=VECTOR('',#14570,1000.);
#3970=VECTOR('',#14573,1000.);
#3971=VECTOR('',#14576,1000.);
#3972=VECTOR('',#14581,35.);
#3973=VECTOR('',#14584,30.);
#3974=VECTOR('',#14589,1000.);
#3975=VECTOR('',#14590,1000.);
#3976=VECTOR('',#14591,1000.);
#3977=VECTOR('',#14594,1000.);
#3978=VECTOR('',#14595,1000.);
#3979=VECTOR('',#14596,1000.);
#3980=VECTOR('',#14599,1000.);
#3981=VECTOR('',#14600,1000.);
#3982=VECTOR('',#14601,1000.);
#3983=VECTOR('',#14604,1000.);
#3984=VECTOR('',#14605,1000.);
#3985=VECTOR('',#14606,1000.);
#3986=VECTOR('',#14609,1000.);
#3987=VECTOR('',#14610,1000.);
#3988=VECTOR('',#14611,1000.);
#3989=VECTOR('',#14614,1000.);
#3990=VECTOR('',#14615,1000.);
#3991=VECTOR('',#14616,1000.);
#3992=VECTOR('',#14619,1000.);
#3993=VECTOR('',#14620,1000.);
#3994=VECTOR('',#14621,1000.);
#3995=VECTOR('',#14624,1000.);
#3996=VECTOR('',#14625,1000.);
#3997=VECTOR('',#14626,1000.);
#3998=VECTOR('',#14629,1000.);
#3999=VECTOR('',#14630,1000.);
#4000=VECTOR('',#14631,1000.);
#4001=VECTOR('',#14634,1000.);
#4002=VECTOR('',#14635,1000.);
#4003=VECTOR('',#14636,1000.);
#4004=VECTOR('',#14639,1000.);
#4005=VECTOR('',#14642,1000.);
#4006=VECTOR('',#14643,1000.);
#4007=VECTOR('',#14644,1000.);
#4008=VECTOR('',#14645,1000.);
#4009=VECTOR('',#14648,1000.);
#4010=VECTOR('',#14649,1000.);
#4011=VECTOR('',#14650,1000.);
#4012=VECTOR('',#14651,1000.);
#4013=VECTOR('',#14654,1000.);
#4014=VECTOR('',#14655,1000.);
#4015=VECTOR('',#14656,1000.);
#4016=VECTOR('',#14657,1000.);
#4017=VECTOR('',#14660,1000.);
#4018=VECTOR('',#14661,1000.);
#4019=VECTOR('',#14662,1000.);
#4020=VECTOR('',#14663,1000.);
#4021=VECTOR('',#14666,1000.);
#4022=VECTOR('',#14667,1000.);
#4023=VECTOR('',#14668,1000.);
#4024=VECTOR('',#14669,1000.);
#4025=VECTOR('',#14672,1000.);
#4026=VECTOR('',#14673,1000.);
#4027=VECTOR('',#14674,1000.);
#4028=VECTOR('',#14675,1000.);
#4029=VECTOR('',#14678,1000.);
#4030=VECTOR('',#14679,1000.);
#4031=VECTOR('',#14680,1000.);
#4032=VECTOR('',#14681,1000.);
#4033=VECTOR('',#14684,1000.);
#4034=VECTOR('',#14685,1000.);
#4035=VECTOR('',#14686,1000.);
#4036=VECTOR('',#14687,1000.);
#4037=VECTOR('',#14690,1000.);
#4038=VECTOR('',#14691,1000.);
#4039=VECTOR('',#14692,1000.);
#4040=VECTOR('',#14693,1000.);
#4041=VECTOR('',#14696,1000.);
#4042=VECTOR('',#14697,1000.);
#4043=VECTOR('',#14698,1000.);
#4044=VECTOR('',#14699,1000.);
#4045=VECTOR('',#14700,1000.);
#4046=VECTOR('',#14701,1000.);
#4047=VECTOR('',#14704,1000.);
#4048=VECTOR('',#14705,1000.);
#4049=VECTOR('',#14706,1000.);
#4050=VECTOR('',#14713,1000.);
#4051=VECTOR('',#14714,1000.);
#4052=VECTOR('',#14715,1000.);
#4053=VECTOR('',#14720,1000.);
#4054=VECTOR('',#14721,1000.);
#4055=VECTOR('',#14724,1000.);
#4056=VECTOR('',#14729,1000.);
#4057=VECTOR('',#14734,1000.);
#4058=VECTOR('',#14739,1000.);
#4059=VECTOR('',#14740,1000.);
#4060=VECTOR('',#14741,1000.);
#4061=VECTOR('',#14746,1000.);
#4062=VECTOR('',#14747,1000.);
#4063=VECTOR('',#14750,1000.);
#4064=VECTOR('',#14755,1000.);
#4065=VECTOR('',#14760,1000.);
#4066=VECTOR('',#14763,1000.);
#4067=VECTOR('',#14764,1000.);
#4068=VECTOR('',#14765,1000.);
#4069=VECTOR('',#14770,1000.);
#4070=VECTOR('',#14771,1000.);
#4071=VECTOR('',#14774,1000.);
#4072=VECTOR('',#14779,1000.);
#4073=VECTOR('',#14784,1000.);
#4074=VECTOR('',#14787,1000.);
#4075=VECTOR('',#14788,1000.);
#4076=VECTOR('',#14789,1000.);
#4077=VECTOR('',#14794,1000.);
#4078=VECTOR('',#14795,1000.);
#4079=VECTOR('',#14798,1000.);
#4080=VECTOR('',#14803,1000.);
#4081=VECTOR('',#14808,1000.);
#4082=VECTOR('',#14811,1000.);
#4083=VECTOR('',#14812,1000.);
#4084=VECTOR('',#14813,1000.);
#4085=VECTOR('',#14818,1000.);
#4086=VECTOR('',#14819,1000.);
#4087=VECTOR('',#14822,1000.);
#4088=VECTOR('',#14827,1000.);
#4089=VECTOR('',#14832,1000.);
#4090=VECTOR('',#14835,1000.);
#4091=VECTOR('',#14836,1000.);
#4092=VECTOR('',#14837,1000.);
#4093=VECTOR('',#14842,1000.);
#4094=VECTOR('',#14843,1000.);
#4095=VECTOR('',#14846,1000.);
#4096=VECTOR('',#14851,1000.);
#4097=VECTOR('',#14856,1000.);
#4098=VECTOR('',#14859,1000.);
#4099=VECTOR('',#14860,1000.);
#4100=VECTOR('',#14861,1000.);
#4101=VECTOR('',#14866,1000.);
#4102=VECTOR('',#14867,1000.);
#4103=VECTOR('',#14870,1000.);
#4104=VECTOR('',#14875,1000.);
#4105=VECTOR('',#14880,1000.);
#4106=VECTOR('',#14883,1000.);
#4107=VECTOR('',#14884,1000.);
#4108=VECTOR('',#14885,1000.);
#4109=VECTOR('',#14890,1000.);
#4110=VECTOR('',#14891,1000.);
#4111=VECTOR('',#14894,1000.);
#4112=VECTOR('',#14899,1000.);
#4113=VECTOR('',#14904,1000.);
#4114=VECTOR('',#14907,1000.);
#4115=VECTOR('',#14908,1000.);
#4116=VECTOR('',#14909,1000.);
#4117=VECTOR('',#14914,1000.);
#4118=VECTOR('',#14915,1000.);
#4119=VECTOR('',#14918,1000.);
#4120=VECTOR('',#14923,1000.);
#4121=VECTOR('',#14928,1000.);
#4122=VECTOR('',#14931,1000.);
#4123=VECTOR('',#14932,1000.);
#4124=VECTOR('',#14933,1000.);
#4125=VECTOR('',#14938,1000.);
#4126=VECTOR('',#14939,1000.);
#4127=VECTOR('',#14942,1000.);
#4128=VECTOR('',#14947,1000.);
#4129=VECTOR('',#14952,1000.);
#4130=VECTOR('',#14995,1000.);
#4131=VECTOR('',#14998,1000.);
#4132=VECTOR('',#15027,6.00000000000001);
#4133=VECTOR('',#15034,5.50000000000001);
#4134=VECTOR('',#15039,6.00000000000001);
#4135=VECTOR('',#15046,5.50000000000001);
#4136=VECTOR('',#15051,6.);
#4137=VECTOR('',#15058,5.49999999999999);
#4138=VECTOR('',#15063,6.00000000000001);
#4139=VECTOR('',#15070,5.50000000000001);
#4140=VECTOR('',#15075,6.00000000000001);
#4141=VECTOR('',#15082,5.49999999999998);
#4142=VECTOR('',#15087,6.);
#4143=VECTOR('',#15094,5.49999999999999);
#4144=VECTOR('',#15099,145.);
#4145=VECTOR('',#15104,195.);
#4146=VECTOR('',#15113,1000.);
#4147=VECTOR('',#15114,1000.);
#4148=VECTOR('',#15115,1000.);
#4149=VECTOR('',#15116,1000.);
#4150=VECTOR('',#15119,1000.);
#4151=VECTOR('',#15120,1000.);
#4152=VECTOR('',#15121,1000.);
#4153=VECTOR('',#15126,1000.);
#4154=VECTOR('',#15131,1000.);
#4155=VECTOR('',#15132,1000.);
#4156=VECTOR('',#15133,1000.);
#4157=VECTOR('',#15138,1000.);
#4158=VECTOR('',#15143,1000.);
#4159=VECTOR('',#15144,1000.);
#4160=VECTOR('',#15145,1000.);
#4161=VECTOR('',#15150,1000.);
#4162=VECTOR('',#15155,1000.);
#4163=VECTOR('',#15156,1000.);
#4164=VECTOR('',#15157,1000.);
#4165=VECTOR('',#15162,1000.);
#4166=VECTOR('',#15167,1000.);
#4167=VECTOR('',#15168,1000.);
#4168=VECTOR('',#15169,1000.);
#4169=VECTOR('',#15172,1000.);
#4170=VECTOR('',#15173,1000.);
#4171=VECTOR('',#15174,1000.);
#4172=VECTOR('',#15177,1000.);
#4173=VECTOR('',#15178,1000.);
#4174=VECTOR('',#15185,1000.);
#4175=VECTOR('',#15188,1000.);
#4176=VECTOR('',#15191,1000.);
#4177=VECTOR('',#15194,1000.);
#4178=VECTOR('',#15197,1000.);
#4179=VECTOR('',#15198,1000.);
#4180=VECTOR('',#15199,1000.);
#4181=VECTOR('',#15200,1000.);
#4182=VECTOR('',#15203,1000.);
#4183=VECTOR('',#15204,1000.);
#4184=VECTOR('',#15205,1000.);
#4185=VECTOR('',#15208,1000.);
#4186=VECTOR('',#15209,1000.);
#4187=VECTOR('',#15212,1000.);
#4188=VECTOR('',#15213,1000.);
#4189=VECTOR('',#15216,1000.);
#4190=VECTOR('',#15221,1000.);
#4191=VECTOR('',#15222,1000.);
#4192=VECTOR('',#15225,1000.);
#4193=VECTOR('',#15230,1000.);
#4194=VECTOR('',#15231,1000.);
#4195=VECTOR('',#15234,1000.);
#4196=VECTOR('',#15239,1000.);
#4197=VECTOR('',#15240,1000.);
#4198=VECTOR('',#15243,1000.);
#4199=VECTOR('',#15248,1000.);
#4200=VECTOR('',#15249,1000.);
#4201=VECTOR('',#15252,1000.);
#4202=VECTOR('',#15257,1000.);
#4203=VECTOR('',#15258,1000.);
#4204=VECTOR('',#15259,1000.);
#4205=VECTOR('',#15260,1000.);
#4206=VECTOR('',#15261,1000.);
#4207=VECTOR('',#15264,1000.);
#4208=VECTOR('',#15267,1000.);
#4209=VECTOR('',#15270,1000.);
#4210=VECTOR('',#15275,1000.);
#4211=VECTOR('',#15276,1000.);
#4212=VECTOR('',#15277,1000.);
#4213=VECTOR('',#15280,1000.);
#4214=VECTOR('',#15281,1000.);
#4215=VECTOR('',#15284,1000.);
#4216=VECTOR('',#15285,1000.);
#4217=VECTOR('',#15290,1000.);
#4218=VECTOR('',#15293,1000.);
#4219=VECTOR('',#15294,1000.);
#4220=VECTOR('',#15299,1000.);
#4221=VECTOR('',#15302,1000.);
#4222=VECTOR('',#15303,1000.);
#4223=VECTOR('',#15308,1000.);
#4224=VECTOR('',#15311,1000.);
#4225=VECTOR('',#15312,1000.);
#4226=VECTOR('',#15317,1000.);
#4227=VECTOR('',#15320,1000.);
#4228=VECTOR('',#15321,1000.);
#4229=VECTOR('',#15324,1000.);
#4230=VECTOR('',#15329,1000.);
#4231=VECTOR('',#15330,1000.);
#4232=VECTOR('',#15331,1000.);
#4233=VECTOR('',#15332,1000.);
#4234=VECTOR('',#15335,1000.);
#4235=VECTOR('',#15336,1000.);
#4236=VECTOR('',#15337,1000.);
#4237=VECTOR('',#15344,1000.);
#4238=VECTOR('',#15347,1000.);
#4239=VECTOR('',#15348,1000.);
#4240=VECTOR('',#15349,1000.);
#4241=VECTOR('',#15356,1000.);
#4242=VECTOR('',#15359,1000.);
#4243=VECTOR('',#15360,1000.);
#4244=VECTOR('',#15361,1000.);
#4245=VECTOR('',#15368,1000.);
#4246=VECTOR('',#15371,1000.);
#4247=VECTOR('',#15372,1000.);
#4248=VECTOR('',#15373,1000.);
#4249=VECTOR('',#15380,1000.);
#4250=VECTOR('',#15383,1000.);
#4251=VECTOR('',#15384,1000.);
#4252=VECTOR('',#15385,1000.);
#4253=VECTOR('',#15388,1000.);
#4254=VECTOR('',#15389,1000.);
#4255=VECTOR('',#15390,1000.);
#4256=VECTOR('',#15393,1000.);
#4257=VECTOR('',#15394,1000.);
#4258=VECTOR('',#15401,1000.);
#4259=VECTOR('',#15402,1000.);
#4260=VECTOR('',#15403,1000.);
#4261=VECTOR('',#15404,1000.);
#4262=VECTOR('',#15407,1000.);
#4263=VECTOR('',#15408,1000.);
#4264=VECTOR('',#15409,1000.);
#4265=VECTOR('',#15414,1000.);
#4266=VECTOR('',#15419,1000.);
#4267=VECTOR('',#15420,1000.);
#4268=VECTOR('',#15421,1000.);
#4269=VECTOR('',#15426,1000.);
#4270=VECTOR('',#15431,1000.);
#4271=VECTOR('',#15432,1000.);
#4272=VECTOR('',#15433,1000.);
#4273=VECTOR('',#15438,1000.);
#4274=VECTOR('',#15443,1000.);
#4275=VECTOR('',#15444,1000.);
#4276=VECTOR('',#15445,1000.);
#4277=VECTOR('',#15450,1000.);
#4278=VECTOR('',#15455,1000.);
#4279=VECTOR('',#15456,1000.);
#4280=VECTOR('',#15457,1000.);
#4281=VECTOR('',#15460,1000.);
#4282=VECTOR('',#15461,1000.);
#4283=VECTOR('',#15462,1000.);
#4284=VECTOR('',#15465,1000.);
#4285=VECTOR('',#15466,1000.);
#4286=VECTOR('',#15473,1000.);
#4287=VECTOR('',#15474,1000.);
#4288=VECTOR('',#15475,1000.);
#4289=VECTOR('',#15476,1000.);
#4290=VECTOR('',#15477,1000.);
#4291=VECTOR('',#15480,1000.);
#4292=VECTOR('',#15483,1000.);
#4293=VECTOR('',#15486,1000.);
#4294=VECTOR('',#15491,1000.);
#4295=VECTOR('',#15492,1000.);
#4296=VECTOR('',#15493,1000.);
#4297=VECTOR('',#15496,1000.);
#4298=VECTOR('',#15497,1000.);
#4299=VECTOR('',#15500,1000.);
#4300=VECTOR('',#15501,1000.);
#4301=VECTOR('',#15506,1000.);
#4302=VECTOR('',#15509,1000.);
#4303=VECTOR('',#15510,1000.);
#4304=VECTOR('',#15515,1000.);
#4305=VECTOR('',#15518,1000.);
#4306=VECTOR('',#15519,1000.);
#4307=VECTOR('',#15524,1000.);
#4308=VECTOR('',#15527,1000.);
#4309=VECTOR('',#15528,1000.);
#4310=VECTOR('',#15533,1000.);
#4311=VECTOR('',#15536,1000.);
#4312=VECTOR('',#15537,1000.);
#4313=VECTOR('',#15540,1000.);
#4314=VECTOR('',#15545,1000.);
#4315=VECTOR('',#15546,1000.);
#4316=VECTOR('',#15547,1000.);
#4317=VECTOR('',#15548,1000.);
#4318=VECTOR('',#15551,1000.);
#4319=VECTOR('',#15552,1000.);
#4320=VECTOR('',#15553,1000.);
#4321=VECTOR('',#15558,1000.);
#4322=VECTOR('',#15563,1000.);
#4323=VECTOR('',#15564,1000.);
#4324=VECTOR('',#15565,1000.);
#4325=VECTOR('',#15570,1000.);
#4326=VECTOR('',#15575,1000.);
#4327=VECTOR('',#15576,1000.);
#4328=VECTOR('',#15577,1000.);
#4329=VECTOR('',#15582,1000.);
#4330=VECTOR('',#15587,1000.);
#4331=VECTOR('',#15588,1000.);
#4332=VECTOR('',#15589,1000.);
#4333=VECTOR('',#15594,1000.);
#4334=VECTOR('',#15599,1000.);
#4335=VECTOR('',#15600,1000.);
#4336=VECTOR('',#15601,1000.);
#4337=VECTOR('',#15604,1000.);
#4338=VECTOR('',#15605,1000.);
#4339=VECTOR('',#15606,1000.);
#4340=VECTOR('',#15609,1000.);
#4341=VECTOR('',#15610,1000.);
#4342=VECTOR('',#15617,1000.);
#4343=VECTOR('',#15618,1000.);
#4344=VECTOR('',#15619,1000.);
#4345=VECTOR('',#15620,1000.);
#4346=VECTOR('',#15621,1000.);
#4347=VECTOR('',#15624,1000.);
#4348=VECTOR('',#15627,1000.);
#4349=VECTOR('',#15630,1000.);
#4350=VECTOR('',#15635,1000.);
#4351=VECTOR('',#15636,1000.);
#4352=VECTOR('',#15637,1000.);
#4353=VECTOR('',#15640,1000.);
#4354=VECTOR('',#15641,1000.);
#4355=VECTOR('',#15644,1000.);
#4356=VECTOR('',#15645,1000.);
#4357=VECTOR('',#15650,1000.);
#4358=VECTOR('',#15653,1000.);
#4359=VECTOR('',#15654,1000.);
#4360=VECTOR('',#15659,1000.);
#4361=VECTOR('',#15662,1000.);
#4362=VECTOR('',#15663,1000.);
#4363=VECTOR('',#15668,1000.);
#4364=VECTOR('',#15671,1000.);
#4365=VECTOR('',#15672,1000.);
#4366=VECTOR('',#15677,1000.);
#4367=VECTOR('',#15680,1000.);
#4368=VECTOR('',#15681,1000.);
#4369=VECTOR('',#15684,1000.);
#4370=VECTOR('',#15689,1000.);
#4371=VECTOR('',#15690,1000.);
#4372=VECTOR('',#15693,1000.);
#4373=VECTOR('',#15696,1000.);
#4374=VECTOR('',#15699,1000.);
#4375=VECTOR('',#15702,1000.);
#4376=VECTOR('',#15703,1000.);
#4377=VECTOR('',#15704,1000.);
#4378=VECTOR('',#15707,1000.);
#4379=VECTOR('',#15708,1000.);
#4380=VECTOR('',#15709,1000.);
#4381=VECTOR('',#15712,1000.);
#4382=VECTOR('',#15713,1000.);
#4383=VECTOR('',#15716,1000.);
#4384=VECTOR('',#15717,1000.);
#4385=VECTOR('',#15720,1000.);
#4386=VECTOR('',#15725,1000.);
#4387=VECTOR('',#15726,1000.);
#4388=VECTOR('',#15729,1000.);
#4389=VECTOR('',#15734,1000.);
#4390=VECTOR('',#15735,1000.);
#4391=VECTOR('',#15738,1000.);
#4392=VECTOR('',#15743,1000.);
#4393=VECTOR('',#15744,1000.);
#4394=VECTOR('',#15747,1000.);
#4395=VECTOR('',#15752,1000.);
#4396=VECTOR('',#15753,1000.);
#4397=VECTOR('',#15756,1000.);
#4398=VECTOR('',#15761,1000.);
#4399=VECTOR('',#15762,1000.);
#4400=VECTOR('',#15763,1000.);
#4401=VECTOR('',#15764,1000.);
#4402=VECTOR('',#15767,1000.);
#4403=VECTOR('',#15770,1000.);
#4404=VECTOR('',#15773,1000.);
#4405=VECTOR('',#15776,1000.);
#4406=VECTOR('',#15779,1000.);
#4407=VECTOR('',#15780,1000.);
#4408=VECTOR('',#15781,1000.);
#4409=VECTOR('',#15784,1000.);
#4410=VECTOR('',#15785,1000.);
#4411=VECTOR('',#15788,1000.);
#4412=VECTOR('',#15789,1000.);
#4413=VECTOR('',#15794,1000.);
#4414=VECTOR('',#15797,1000.);
#4415=VECTOR('',#15798,1000.);
#4416=VECTOR('',#15803,1000.);
#4417=VECTOR('',#15806,1000.);
#4418=VECTOR('',#15807,1000.);
#4419=VECTOR('',#15812,1000.);
#4420=VECTOR('',#15815,1000.);
#4421=VECTOR('',#15816,1000.);
#4422=VECTOR('',#15821,1000.);
#4423=VECTOR('',#15824,1000.);
#4424=VECTOR('',#15825,1000.);
#4425=VECTOR('',#15828,1000.);
#4426=VECTOR('',#15833,1000.);
#4427=VECTOR('',#15834,1000.);
#4428=VECTOR('',#15835,1000.);
#4429=VECTOR('',#15836,1000.);
#4430=VECTOR('',#15839,1000.);
#4431=VECTOR('',#15840,1000.);
#4432=VECTOR('',#15841,1000.);
#4433=VECTOR('',#15846,1000.);
#4434=VECTOR('',#15851,1000.);
#4435=VECTOR('',#15852,1000.);
#4436=VECTOR('',#15853,1000.);
#4437=VECTOR('',#15858,1000.);
#4438=VECTOR('',#15863,1000.);
#4439=VECTOR('',#15864,1000.);
#4440=VECTOR('',#15865,1000.);
#4441=VECTOR('',#15870,1000.);
#4442=VECTOR('',#15875,1000.);
#4443=VECTOR('',#15876,1000.);
#4444=VECTOR('',#15877,1000.);
#4445=VECTOR('',#15880,1000.);
#4446=VECTOR('',#15881,1000.);
#4447=VECTOR('',#15888,1000.);
#4448=VECTOR('',#15889,1000.);
#4449=VECTOR('',#15890,1000.);
#4450=VECTOR('',#15891,1000.);
#4451=VECTOR('',#15894,1000.);
#4452=VECTOR('',#15895,1000.);
#4453=VECTOR('',#15896,1000.);
#4454=VECTOR('',#15901,1000.);
#4455=VECTOR('',#15906,1000.);
#4456=VECTOR('',#15907,1000.);
#4457=VECTOR('',#15908,1000.);
#4458=VECTOR('',#15913,1000.);
#4459=VECTOR('',#15918,1000.);
#4460=VECTOR('',#15919,1000.);
#4461=VECTOR('',#15920,1000.);
#4462=VECTOR('',#15925,1000.);
#4463=VECTOR('',#15930,1000.);
#4464=VECTOR('',#15931,1000.);
#4465=VECTOR('',#15932,1000.);
#4466=VECTOR('',#15935,1000.);
#4467=VECTOR('',#15936,1000.);
#4468=VECTOR('',#15943,1000.);
#4469=VECTOR('',#15944,1000.);
#4470=VECTOR('',#15945,1000.);
#4471=VECTOR('',#15946,1000.);
#4472=VECTOR('',#15949,1000.);
#4473=VECTOR('',#15950,1000.);
#4474=VECTOR('',#15951,1000.);
#4475=VECTOR('',#15958,1000.);
#4476=VECTOR('',#15961,1000.);
#4477=VECTOR('',#15962,1000.);
#4478=VECTOR('',#15963,1000.);
#4479=VECTOR('',#15970,1000.);
#4480=VECTOR('',#15973,1000.);
#4481=VECTOR('',#15974,1000.);
#4482=VECTOR('',#15975,1000.);
#4483=VECTOR('',#15982,1000.);
#4484=VECTOR('',#15985,1000.);
#4485=VECTOR('',#15986,1000.);
#4486=VECTOR('',#15987,1000.);
#4487=VECTOR('',#15990,1000.);
#4488=VECTOR('',#15991,1000.);
#4489=VECTOR('',#15998,1000.);
#4490=VECTOR('',#15999,1000.);
#4491=VECTOR('',#16000,1000.);
#4492=VECTOR('',#16001,1000.);
#4493=VECTOR('',#16004,1000.);
#4494=VECTOR('',#16005,1000.);
#4495=VECTOR('',#16006,1000.);
#4496=VECTOR('',#16013,1000.);
#4497=VECTOR('',#16016,1000.);
#4498=VECTOR('',#16017,1000.);
#4499=VECTOR('',#16018,1000.);
#4500=VECTOR('',#16025,1000.);
#4501=VECTOR('',#16028,1000.);
#4502=VECTOR('',#16029,1000.);
#4503=VECTOR('',#16030,1000.);
#4504=VECTOR('',#16037,1000.);
#4505=VECTOR('',#16040,1000.);
#4506=VECTOR('',#16041,1000.);
#4507=VECTOR('',#16042,1000.);
#4508=VECTOR('',#16045,1000.);
#4509=VECTOR('',#16046,1000.);
#4510=VECTOR('',#16053,1000.);
#4511=VECTOR('',#16054,1000.);
#4512=VECTOR('',#16057,1000.);
#4513=VECTOR('',#16060,1000.);
#4514=VECTOR('',#16063,1000.);
#4515=VECTOR('',#16064,1000.);
#4516=VECTOR('',#16067,1000.);
#4517=VECTOR('',#16068,1000.);
#4518=VECTOR('',#16069,1000.);
#4519=VECTOR('',#16072,1000.);
#4520=VECTOR('',#16073,1000.);
#4521=VECTOR('',#16076,1000.);
#4522=VECTOR('',#16081,1000.);
#4523=VECTOR('',#16082,1000.);
#4524=VECTOR('',#16085,1000.);
#4525=VECTOR('',#16090,1000.);
#4526=VECTOR('',#16091,1000.);
#4527=VECTOR('',#16094,1000.);
#4528=VECTOR('',#16099,1000.);
#4529=VECTOR('',#16100,1000.);
#4530=VECTOR('',#16103,1000.);
#4531=VECTOR('',#16108,1000.);
#4532=VECTOR('',#16109,1000.);
#4533=VECTOR('',#16110,1000.);
#4534=VECTOR('',#16111,1000.);
#4535=VECTOR('',#16114,1000.);
#4536=VECTOR('',#16115,1000.);
#4537=VECTOR('',#16116,1000.);
#4538=VECTOR('',#16121,1000.);
#4539=VECTOR('',#16126,1000.);
#4540=VECTOR('',#16127,1000.);
#4541=VECTOR('',#16128,1000.);
#4542=VECTOR('',#16133,1000.);
#4543=VECTOR('',#16138,1000.);
#4544=VECTOR('',#16139,1000.);
#4545=VECTOR('',#16140,1000.);
#4546=VECTOR('',#16145,1000.);
#4547=VECTOR('',#16150,1000.);
#4548=VECTOR('',#16151,1000.);
#4549=VECTOR('',#16152,1000.);
#4550=VECTOR('',#16155,1000.);
#4551=VECTOR('',#16156,1000.);
#4552=VECTOR('',#16163,1000.);
#4553=VECTOR('',#16164,1000.);
#4554=VECTOR('',#16165,1000.);
#4555=VECTOR('',#16168,1000.);
#4556=VECTOR('',#16171,1000.);
#4557=VECTOR('',#16174,1000.);
#4558=VECTOR('',#16177,1000.);
#4559=VECTOR('',#16178,1000.);
#4560=VECTOR('',#16179,1000.);
#4561=VECTOR('',#16182,1000.);
#4562=VECTOR('',#16183,1000.);
#4563=VECTOR('',#16188,1000.);
#4564=VECTOR('',#16191,1000.);
#4565=VECTOR('',#16192,1000.);
#4566=VECTOR('',#16197,1000.);
#4567=VECTOR('',#16200,1000.);
#4568=VECTOR('',#16201,1000.);
#4569=VECTOR('',#16206,1000.);
#4570=VECTOR('',#16209,1000.);
#4571=VECTOR('',#16210,1000.);
#4572=VECTOR('',#16213,1000.);
#4573=VECTOR('',#16218,1000.);
#4574=VECTOR('',#16219,1000.);
#4575=VECTOR('',#16220,1000.);
#4576=VECTOR('',#16223,1000.);
#4577=VECTOR('',#16226,1000.);
#4578=VECTOR('',#16229,1000.);
#4579=VECTOR('',#16232,1000.);
#4580=VECTOR('',#16233,1000.);
#4581=VECTOR('',#16234,1000.);
#4582=VECTOR('',#16237,1000.);
#4583=VECTOR('',#16238,1000.);
#4584=VECTOR('',#16243,1000.);
#4585=VECTOR('',#16246,1000.);
#4586=VECTOR('',#16247,1000.);
#4587=VECTOR('',#16252,1000.);
#4588=VECTOR('',#16255,1000.);
#4589=VECTOR('',#16256,1000.);
#4590=VECTOR('',#16261,1000.);
#4591=VECTOR('',#16264,1000.);
#4592=VECTOR('',#16265,1000.);
#4593=VECTOR('',#16268,1000.);
#4594=VECTOR('',#16273,1000.);
#4595=VECTOR('',#16274,1000.);
#4596=VECTOR('',#16275,1000.);
#4597=VECTOR('',#16276,1000.);
#4598=VECTOR('',#16279,1000.);
#4599=VECTOR('',#16280,1000.);
#4600=VECTOR('',#16281,1000.);
#4601=VECTOR('',#16288,1000.);
#4602=VECTOR('',#16291,1000.);
#4603=VECTOR('',#16292,1000.);
#4604=VECTOR('',#16293,1000.);
#4605=VECTOR('',#16300,1000.);
#4606=VECTOR('',#16303,1000.);
#4607=VECTOR('',#16304,1000.);
#4608=VECTOR('',#16305,1000.);
#4609=VECTOR('',#16312,1000.);
#4610=VECTOR('',#16315,1000.);
#4611=VECTOR('',#16316,1000.);
#4612=VECTOR('',#16317,1000.);
#4613=VECTOR('',#16320,1000.);
#4614=VECTOR('',#16321,1000.);
#4615=VECTOR('',#16328,1000.);
#4616=VECTOR('',#16329,1000.);
#4617=VECTOR('',#16332,1000.);
#4618=VECTOR('',#16335,1000.);
#4619=VECTOR('',#16338,1000.);
#4620=VECTOR('',#16339,1000.);
#4621=VECTOR('',#16342,1000.);
#4622=VECTOR('',#16343,1000.);
#4623=VECTOR('',#16344,1000.);
#4624=VECTOR('',#16347,1000.);
#4625=VECTOR('',#16348,1000.);
#4626=VECTOR('',#16351,1000.);
#4627=VECTOR('',#16356,1000.);
#4628=VECTOR('',#16357,1000.);
#4629=VECTOR('',#16360,1000.);
#4630=VECTOR('',#16365,1000.);
#4631=VECTOR('',#16366,1000.);
#4632=VECTOR('',#16369,1000.);
#4633=VECTOR('',#16374,1000.);
#4634=VECTOR('',#16375,1000.);
#4635=VECTOR('',#16378,1000.);
#4636=VECTOR('',#16385,1000.);
#4637=VECTOR('',#16388,1000.);
#4638=VECTOR('',#16393,1000.);
#4639=VECTOR('',#16396,1000.);
#4640=VECTOR('',#16401,1000.);
#4641=VECTOR('',#16404,1000.);
#4642=VECTOR('',#16409,1000.);
#4643=VECTOR('',#16412,1000.);
#4644=VECTOR('',#16415,1000.);
#4645=VECTOR('',#16416,1000.);
#4646=VECTOR('',#16417,1000.);
#4647=VECTOR('',#16418,1000.);
#4648=VECTOR('',#16421,1000.);
#4649=VECTOR('',#16422,1000.);
#4650=VECTOR('',#16423,1000.);
#4651=VECTOR('',#16424,1000.);
#4652=VECTOR('',#16427,1000.);
#4653=VECTOR('',#16428,1000.);
#4654=VECTOR('',#16429,1000.);
#4655=VECTOR('',#16430,1000.);
#4656=VECTOR('',#16433,1000.);
#4657=VECTOR('',#16434,1000.);
#4658=VECTOR('',#16435,1000.);
#4659=VECTOR('',#16436,1000.);
#4660=VECTOR('',#16439,1000.);
#4661=VECTOR('',#16440,1000.);
#4662=VECTOR('',#16441,1000.);
#4663=VECTOR('',#16442,1000.);
#4664=VECTOR('',#16443,1000.);
#4665=VECTOR('',#16444,1000.);
#4666=VECTOR('',#16447,1000.);
#4667=VECTOR('',#16448,1000.);
#4668=VECTOR('',#16451,1000.);
#4669=VECTOR('',#16452,1000.);
#4670=VECTOR('',#16455,1000.);
#4671=VECTOR('',#16456,1000.);
#4672=VECTOR('',#16461,1000.);
#4673=VECTOR('',#16462,1000.);
#4674=VECTOR('',#16463,1000.);
#4675=VECTOR('',#16464,1000.);
#4676=VECTOR('',#16465,1000.);
#4677=VECTOR('',#16468,1000.);
#4678=VECTOR('',#16469,1000.);
#4679=VECTOR('',#16472,1000.);
#4680=VECTOR('',#16473,1000.);
#4681=VECTOR('',#16476,1000.);
#4682=VECTOR('',#16477,1000.);
#4683=VECTOR('',#16480,1000.);
#4684=VECTOR('',#16483,1000.);
#4685=VECTOR('',#16486,1000.);
#4686=VECTOR('',#16491,1000.);
#4687=VECTOR('',#16494,1000.);
#4688=VECTOR('',#16499,1000.);
#4689=VECTOR('',#16502,1000.);
#4690=VECTOR('',#16507,1000.);
#4691=VECTOR('',#16510,1000.);
#4692=VECTOR('',#16525,8.74999999999998);
#4693=VECTOR('',#16532,8.74999999999998);
#4694=VECTOR('',#16537,1000.);
#4695=VECTOR('',#16538,1000.);
#4696=VECTOR('',#16539,1000.);
#4697=VECTOR('',#16540,1000.);
#4698=VECTOR('',#16543,1000.);
#4699=VECTOR('',#16544,1000.);
#4700=VECTOR('',#16545,1000.);
#4701=VECTOR('',#16550,1000.);
#4702=VECTOR('',#16555,1000.);
#4703=VECTOR('',#16556,1000.);
#4704=VECTOR('',#16557,1000.);
#4705=VECTOR('',#16562,1000.);
#4706=VECTOR('',#16567,1000.);
#4707=VECTOR('',#16568,1000.);
#4708=VECTOR('',#16569,1000.);
#4709=VECTOR('',#16574,1000.);
#4710=VECTOR('',#16579,1000.);
#4711=VECTOR('',#16580,1000.);
#4712=VECTOR('',#16581,1000.);
#4713=VECTOR('',#16586,1000.);
#4714=VECTOR('',#16591,1000.);
#4715=VECTOR('',#16592,1000.);
#4716=VECTOR('',#16593,1000.);
#4717=VECTOR('',#16596,1000.);
#4718=VECTOR('',#16597,1000.);
#4719=VECTOR('',#16598,1000.);
#4720=VECTOR('',#16601,1000.);
#4721=VECTOR('',#16602,1000.);
#4722=VECTOR('',#16611,4.5);
#4723=VECTOR('',#16618,4.5);
#4724=VECTOR('',#16623,1000.);
#4725=VECTOR('',#16624,1000.);
#4726=VECTOR('',#16625,1000.);
#4727=VECTOR('',#16626,1000.);
#4728=VECTOR('',#16629,1000.);
#4729=VECTOR('',#16630,1000.);
#4730=VECTOR('',#16631,1000.);
#4731=VECTOR('',#16636,1000.);
#4732=VECTOR('',#16641,1000.);
#4733=VECTOR('',#16642,1000.);
#4734=VECTOR('',#16643,1000.);
#4735=VECTOR('',#16648,1000.);
#4736=VECTOR('',#16653,1000.);
#4737=VECTOR('',#16654,1000.);
#4738=VECTOR('',#16655,1000.);
#4739=VECTOR('',#16660,1000.);
#4740=VECTOR('',#16665,1000.);
#4741=VECTOR('',#16666,1000.);
#4742=VECTOR('',#16667,1000.);
#4743=VECTOR('',#16670,1000.);
#4744=VECTOR('',#16671,1000.);
#4745=VECTOR('',#16680,4.5);
#4746=VECTOR('',#16687,4.5);
#4747=VECTOR('',#16692,1000.);
#4748=VECTOR('',#16693,1000.);
#4749=VECTOR('',#16694,1000.);
#4750=VECTOR('',#16695,1000.);
#4751=VECTOR('',#16698,1000.);
#4752=VECTOR('',#16699,1000.);
#4753=VECTOR('',#16700,1000.);
#4754=VECTOR('',#16707,1000.);
#4755=VECTOR('',#16710,1000.);
#4756=VECTOR('',#16711,1000.);
#4757=VECTOR('',#16712,1000.);
#4758=VECTOR('',#16719,1000.);
#4759=VECTOR('',#16722,1000.);
#4760=VECTOR('',#16723,1000.);
#4761=VECTOR('',#16724,1000.);
#4762=VECTOR('',#16731,1000.);
#4763=VECTOR('',#16734,1000.);
#4764=VECTOR('',#16735,1000.);
#4765=VECTOR('',#16736,1000.);
#4766=VECTOR('',#16739,1000.);
#4767=VECTOR('',#16740,1000.);
#4768=VERTEX_POINT('',#16756);
#4769=VERTEX_POINT('',#16757);
#4770=VERTEX_POINT('',#16759);
#4771=VERTEX_POINT('',#16808);
#4772=VERTEX_POINT('',#16809);
#4773=VERTEX_POINT('',#16812);
#4774=VERTEX_POINT('',#16816);
#4775=VERTEX_POINT('',#16817);
#4776=VERTEX_POINT('',#16819);
#4777=VERTEX_POINT('',#16821);
#4778=VERTEX_POINT('',#16825);
#4779=VERTEX_POINT('',#16826);
#4780=VERTEX_POINT('',#16828);
#4781=VERTEX_POINT('',#16830);
#4782=VERTEX_POINT('',#16832);
#4783=VERTEX_POINT('',#16836);
#4784=VERTEX_POINT('',#16837);
#4785=VERTEX_POINT('',#16839);
#4786=VERTEX_POINT('',#16841);
#4787=VERTEX_POINT('',#16845);
#4788=VERTEX_POINT('',#16846);
#4789=VERTEX_POINT('',#16848);
#4790=VERTEX_POINT('',#16852);
#4791=VERTEX_POINT('',#16853);
#4792=VERTEX_POINT('',#16855);
#4793=VERTEX_POINT('',#16859);
#4794=VERTEX_POINT('',#16860);
#4795=VERTEX_POINT('',#16862);
#4796=VERTEX_POINT('',#16866);
#4797=VERTEX_POINT('',#16867);
#4798=VERTEX_POINT('',#16869);
#4799=VERTEX_POINT('',#16873);
#4800=VERTEX_POINT('',#16875);
#4801=VERTEX_POINT('',#16877);
#4802=VERTEX_POINT('',#16881);
#4803=VERTEX_POINT('',#16882);
#4804=VERTEX_POINT('',#16885);
#4805=VERTEX_POINT('',#16889);
#4806=VERTEX_POINT('',#16891);
#4807=VERTEX_POINT('',#16895);
#4808=VERTEX_POINT('',#16899);
#4809=VERTEX_POINT('',#16901);
#4810=VERTEX_POINT('',#16905);
#4811=VERTEX_POINT('',#16909);
#4812=VERTEX_POINT('',#16911);
#4813=VERTEX_POINT('',#16915);
#4814=VERTEX_POINT('',#16919);
#4815=VERTEX_POINT('',#16921);
#4816=VERTEX_POINT('',#16925);
#4817=VERTEX_POINT('',#16929);
#4818=VERTEX_POINT('',#16931);
#4819=VERTEX_POINT('',#16935);
#4820=VERTEX_POINT('',#16939);
#4821=VERTEX_POINT('',#16941);
#4822=VERTEX_POINT('',#16945);
#4823=VERTEX_POINT('',#16951);
#4824=VERTEX_POINT('',#16953);
#4825=VERTEX_POINT('',#16957);
#4826=VERTEX_POINT('',#16958);
#4827=VERTEX_POINT('',#16961);
#4828=VERTEX_POINT('',#16967);
#4829=VERTEX_POINT('',#16969);
#4830=VERTEX_POINT('',#16973);
#4831=VERTEX_POINT('',#16975);
#4832=VERTEX_POINT('',#16979);
#4833=VERTEX_POINT('',#16981);
#4834=VERTEX_POINT('',#16985);
#4835=VERTEX_POINT('',#16987);
#4836=VERTEX_POINT('',#16991);
#4837=VERTEX_POINT('',#16992);
#4838=VERTEX_POINT('',#16994);
#4839=VERTEX_POINT('',#16996);
#4840=VERTEX_POINT('',#17000);
#4841=VERTEX_POINT('',#17153);
#4842=VERTEX_POINT('',#17302);
#4843=VERTEX_POINT('',#17304);
#4844=VERTEX_POINT('',#17351);
#4845=VERTEX_POINT('',#17356);
#4846=VERTEX_POINT('',#17357);
#4847=VERTEX_POINT('',#17359);
#4848=VERTEX_POINT('',#17361);
#4849=VERTEX_POINT('',#17363);
#4850=VERTEX_POINT('',#17365);
#4851=VERTEX_POINT('',#17369);
#4852=VERTEX_POINT('',#17371);
#4853=VERTEX_POINT('',#17373);
#4854=VERTEX_POINT('',#17376);
#4855=VERTEX_POINT('',#17423);
#4856=VERTEX_POINT('',#17573);
#4857=VERTEX_POINT('',#17740);
#4858=VERTEX_POINT('',#17788);
#4859=VERTEX_POINT('',#17790);
#4860=VERTEX_POINT('',#17876);
#4861=VERTEX_POINT('',#17878);
#4862=VERTEX_POINT('',#17959);
#4863=VERTEX_POINT('',#18045);
#4864=VERTEX_POINT('',#18047);
#4865=VERTEX_POINT('',#18127);
#4866=VERTEX_POINT('',#18129);
#4867=VERTEX_POINT('',#18206);
#4868=VERTEX_POINT('',#18290);
#4869=VERTEX_POINT('',#18292);
#4870=VERTEX_POINT('',#18378);
#4871=VERTEX_POINT('',#18380);
#4872=VERTEX_POINT('',#18461);
#4873=VERTEX_POINT('',#18463);
#4874=VERTEX_POINT('',#18549);
#4875=VERTEX_POINT('',#18551);
#4876=VERTEX_POINT('',#18633);
#4877=VERTEX_POINT('',#18635);
#4878=VERTEX_POINT('',#18721);
#4879=VERTEX_POINT('',#18723);
#4880=VERTEX_POINT('',#18804);
#4881=VERTEX_POINT('',#18806);
#4882=VERTEX_POINT('',#18892);
#4883=VERTEX_POINT('',#18894);
#4884=VERTEX_POINT('',#18974);
#4885=VERTEX_POINT('',#18976);
#4886=VERTEX_POINT('',#19053);
#4887=VERTEX_POINT('',#19055);
#4888=VERTEX_POINT('',#19140);
#4889=VERTEX_POINT('',#19141);
#4890=VERTEX_POINT('',#19143);
#4891=VERTEX_POINT('',#19145);
#4892=VERTEX_POINT('',#19147);
#4893=VERTEX_POINT('',#19149);
#4894=VERTEX_POINT('',#19153);
#4895=VERTEX_POINT('',#19154);
#4896=VERTEX_POINT('',#19156);
#4897=VERTEX_POINT('',#19158);
#4898=VERTEX_POINT('',#19160);
#4899=VERTEX_POINT('',#19163);
#4900=VERTEX_POINT('',#19165);
#4901=VERTEX_POINT('',#19167);
#4902=VERTEX_POINT('',#19169);
#4903=VERTEX_POINT('',#19173);
#4904=VERTEX_POINT('',#19175);
#4905=VERTEX_POINT('',#19177);
#4906=VERTEX_POINT('',#19179);
#4907=VERTEX_POINT('',#19182);
#4908=VERTEX_POINT('',#19186);
#4909=VERTEX_POINT('',#19188);
#4910=VERTEX_POINT('',#19190);
#4911=VERTEX_POINT('',#19192);
#4912=VERTEX_POINT('',#19194);
#4913=VERTEX_POINT('',#19197);
#4914=VERTEX_POINT('',#19199);
#4915=VERTEX_POINT('',#19201);
#4916=VERTEX_POINT('',#19203);
#4917=VERTEX_POINT('',#19206);
#4918=VERTEX_POINT('',#19208);
#4919=VERTEX_POINT('',#19210);
#4920=VERTEX_POINT('',#19215);
#4921=VERTEX_POINT('',#19217);
#4922=VERTEX_POINT('',#19221);
#4923=VERTEX_POINT('',#19222);
#4924=VERTEX_POINT('',#19224);
#4925=VERTEX_POINT('',#19226);
#4926=VERTEX_POINT('',#19228);
#4927=VERTEX_POINT('',#19232);
#4928=VERTEX_POINT('',#19234);
#4929=VERTEX_POINT('',#19236);
#4930=VERTEX_POINT('',#19238);
#4931=VERTEX_POINT('',#19242);
#4932=VERTEX_POINT('',#19243);
#4933=VERTEX_POINT('',#19245);
#4934=VERTEX_POINT('',#19247);
#4935=VERTEX_POINT('',#19249);
#4936=VERTEX_POINT('',#19253);
#4937=VERTEX_POINT('',#19254);
#4938=VERTEX_POINT('',#19256);
#4939=VERTEX_POINT('',#19258);
#4940=VERTEX_POINT('',#19260);
#4941=VERTEX_POINT('',#19262);
#4942=VERTEX_POINT('',#19264);
#4943=VERTEX_POINT('',#19266);
#4944=VERTEX_POINT('',#19269);
#4945=VERTEX_POINT('',#19270);
#4946=VERTEX_POINT('',#19272);
#4947=VERTEX_POINT('',#19274);
#4948=VERTEX_POINT('',#19276);
#4949=VERTEX_POINT('',#19278);
#4950=VERTEX_POINT('',#19280);
#4951=VERTEX_POINT('',#19282);
#4952=VERTEX_POINT('',#19286);
#4953=VERTEX_POINT('',#19289);
#4954=VERTEX_POINT('',#19293);
#4955=VERTEX_POINT('',#19295);
#4956=VERTEX_POINT('',#19297);
#4957=VERTEX_POINT('',#19301);
#4958=VERTEX_POINT('',#19302);
#4959=VERTEX_POINT('',#19304);
#4960=VERTEX_POINT('',#19309);
#4961=VERTEX_POINT('',#19311);
#4962=VERTEX_POINT('',#19328);
#4963=VERTEX_POINT('',#19332);
#4964=VERTEX_POINT('',#19333);
#4965=VERTEX_POINT('',#19348);
#4966=VERTEX_POINT('',#19350);
#4967=VERTEX_POINT('',#19380);
#4968=VERTEX_POINT('',#20727);
#4969=VERTEX_POINT('',#20729);
#4970=VERTEX_POINT('',#20733);
#4971=VERTEX_POINT('',#20734);
#4972=VERTEX_POINT('',#20736);
#4973=VERTEX_POINT('',#20738);
#4974=VERTEX_POINT('',#20740);
#4975=VERTEX_POINT('',#20744);
#4976=VERTEX_POINT('',#20746);
#4977=VERTEX_POINT('',#20748);
#4978=VERTEX_POINT('',#20750);
#4979=VERTEX_POINT('',#20754);
#4980=VERTEX_POINT('',#20755);
#4981=VERTEX_POINT('',#20757);
#4982=VERTEX_POINT('',#20759);
#4983=VERTEX_POINT('',#20761);
#4984=VERTEX_POINT('',#20765);
#4985=VERTEX_POINT('',#20768);
#4986=VERTEX_POINT('',#20772);
#4987=VERTEX_POINT('',#20774);
#4988=VERTEX_POINT('',#20776);
#4989=VERTEX_POINT('',#20780);
#4990=VERTEX_POINT('',#20781);
#4991=VERTEX_POINT('',#20784);
#4992=VERTEX_POINT('',#20788);
#4993=VERTEX_POINT('',#20790);
#4994=VERTEX_POINT('',#20794);
#4995=VERTEX_POINT('',#20808);
#4996=VERTEX_POINT('',#20809);
#4997=VERTEX_POINT('',#20821);
#4998=VERTEX_POINT('',#20823);
#4999=VERTEX_POINT('',#20837);
#5000=VERTEX_POINT('',#22252);
#5001=VERTEX_POINT('',#22253);
#5002=VERTEX_POINT('',#22255);
#5003=VERTEX_POINT('',#22257);
#5004=VERTEX_POINT('',#22261);
#5005=VERTEX_POINT('',#22262);
#5006=VERTEX_POINT('',#22264);
#5007=VERTEX_POINT('',#22266);
#5008=VERTEX_POINT('',#22268);
#5009=VERTEX_POINT('',#22270);
#5010=VERTEX_POINT('',#22274);
#5011=VERTEX_POINT('',#22275);
#5012=VERTEX_POINT('',#22277);
#5013=VERTEX_POINT('',#22279);
#5014=VERTEX_POINT('',#22283);
#5015=VERTEX_POINT('',#22284);
#5016=VERTEX_POINT('',#22286);
#5017=VERTEX_POINT('',#22288);
#5018=VERTEX_POINT('',#22292);
#5019=VERTEX_POINT('',#22293);
#5020=VERTEX_POINT('',#22295);
#5021=VERTEX_POINT('',#22297);
#5022=VERTEX_POINT('',#22301);
#5023=VERTEX_POINT('',#22302);
#5024=VERTEX_POINT('',#22304);
#5025=VERTEX_POINT('',#22308);
#5026=VERTEX_POINT('',#22309);
#5027=VERTEX_POINT('',#22311);
#5028=VERTEX_POINT('',#22315);
#5029=VERTEX_POINT('',#22316);
#5030=VERTEX_POINT('',#22318);
#5031=VERTEX_POINT('',#22320);
#5032=VERTEX_POINT('',#22324);
#5033=VERTEX_POINT('',#22325);
#5034=VERTEX_POINT('',#22327);
#5035=VERTEX_POINT('',#22331);
#5036=VERTEX_POINT('',#22332);
#5037=VERTEX_POINT('',#22334);
#5038=VERTEX_POINT('',#22338);
#5039=VERTEX_POINT('',#22339);
#5040=VERTEX_POINT('',#22341);
#5041=VERTEX_POINT('',#22343);
#5042=VERTEX_POINT('',#22347);
#5043=VERTEX_POINT('',#22348);
#5044=VERTEX_POINT('',#22350);
#5045=VERTEX_POINT('',#22352);
#5046=VERTEX_POINT('',#22356);
#5047=VERTEX_POINT('',#22357);
#5048=VERTEX_POINT('',#22359);
#5049=VERTEX_POINT('',#22361);
#5050=VERTEX_POINT('',#22365);
#5051=VERTEX_POINT('',#22366);
#5052=VERTEX_POINT('',#22368);
#5053=VERTEX_POINT('',#22370);
#5054=VERTEX_POINT('',#22374);
#5055=VERTEX_POINT('',#22375);
#5056=VERTEX_POINT('',#22380);
#5057=VERTEX_POINT('',#22382);
#5058=VERTEX_POINT('',#22386);
#5059=VERTEX_POINT('',#22387);
#5060=VERTEX_POINT('',#22389);
#5061=VERTEX_POINT('',#22391);
#5062=VERTEX_POINT('',#22395);
#5063=VERTEX_POINT('',#22397);
#5064=VERTEX_POINT('',#22401);
#5065=VERTEX_POINT('',#22402);
#5066=VERTEX_POINT('',#22407);
#5067=VERTEX_POINT('',#22408);
#5068=VERTEX_POINT('',#22410);
#5069=VERTEX_POINT('',#22412);
#5070=VERTEX_POINT('',#22416);
#5071=VERTEX_POINT('',#22417);
#5072=VERTEX_POINT('',#22419);
#5073=VERTEX_POINT('',#22421);
#5074=VERTEX_POINT('',#22425);
#5075=VERTEX_POINT('',#22426);
#5076=VERTEX_POINT('',#22428);
#5077=VERTEX_POINT('',#22430);
#5078=VERTEX_POINT('',#22434);
#5079=VERTEX_POINT('',#22435);
#5080=VERTEX_POINT('',#22437);
#5081=VERTEX_POINT('',#22439);
#5082=VERTEX_POINT('',#25205);
#5083=VERTEX_POINT('',#25207);
#5084=VERTEX_POINT('',#25209);
#5085=VERTEX_POINT('',#25213);
#5086=VERTEX_POINT('',#25214);
#5087=VERTEX_POINT('',#25217);
#5088=VERTEX_POINT('',#25221);
#5089=VERTEX_POINT('',#25222);
#5090=VERTEX_POINT('',#25225);
#5091=VERTEX_POINT('',#25229);
#5092=VERTEX_POINT('',#25230);
#5093=VERTEX_POINT('',#25232);
#5094=VERTEX_POINT('',#25234);
#5095=VERTEX_POINT('',#25238);
#5096=VERTEX_POINT('',#25240);
#5097=VERTEX_POINT('',#25242);
#5098=VERTEX_POINT('',#25244);
#5099=VERTEX_POINT('',#25246);
#5100=VERTEX_POINT('',#25248);
#5101=VERTEX_POINT('',#25250);
#5102=VERTEX_POINT('',#25252);
#5103=VERTEX_POINT('',#25254);
#5104=VERTEX_POINT('',#25256);
#5105=VERTEX_POINT('',#25258);
#5106=VERTEX_POINT('',#25260);
#5107=VERTEX_POINT('',#25262);
#5108=VERTEX_POINT('',#25264);
#5109=VERTEX_POINT('',#25266);
#5110=VERTEX_POINT('',#25268);
#5111=VERTEX_POINT('',#25270);
#5112=VERTEX_POINT('',#25272);
#5113=VERTEX_POINT('',#25274);
#5114=VERTEX_POINT('',#25276);
#5115=VERTEX_POINT('',#25278);
#5116=VERTEX_POINT('',#25280);
#5117=VERTEX_POINT('',#25284);
#5118=VERTEX_POINT('',#25286);
#5119=VERTEX_POINT('',#25288);
#5120=VERTEX_POINT('',#25290);
#5121=VERTEX_POINT('',#25292);
#5122=VERTEX_POINT('',#25294);
#5123=VERTEX_POINT('',#25297);
#5124=VERTEX_POINT('',#25299);
#5125=VERTEX_POINT('',#25302);
#5126=VERTEX_POINT('',#25303);
#5127=VERTEX_POINT('',#25305);
#5128=VERTEX_POINT('',#25307);
#5129=VERTEX_POINT('',#25310);
#5130=VERTEX_POINT('',#25311);
#5131=VERTEX_POINT('',#25313);
#5132=VERTEX_POINT('',#25315);
#5133=VERTEX_POINT('',#25318);
#5134=VERTEX_POINT('',#25319);
#5135=VERTEX_POINT('',#25321);
#5136=VERTEX_POINT('',#25323);
#5137=VERTEX_POINT('',#25326);
#5138=VERTEX_POINT('',#25327);
#5139=VERTEX_POINT('',#25329);
#5140=VERTEX_POINT('',#25331);
#5141=VERTEX_POINT('',#25334);
#5142=VERTEX_POINT('',#25335);
#5143=VERTEX_POINT('',#25337);
#5144=VERTEX_POINT('',#25339);
#5145=VERTEX_POINT('',#25342);
#5146=VERTEX_POINT('',#25343);
#5147=VERTEX_POINT('',#25345);
#5148=VERTEX_POINT('',#25347);
#5149=VERTEX_POINT('',#25350);
#5150=VERTEX_POINT('',#25351);
#5151=VERTEX_POINT('',#25353);
#5152=VERTEX_POINT('',#25355);
#5153=VERTEX_POINT('',#25358);
#5154=VERTEX_POINT('',#25359);
#5155=VERTEX_POINT('',#25361);
#5156=VERTEX_POINT('',#25363);
#5157=VERTEX_POINT('',#25366);
#5158=VERTEX_POINT('',#25367);
#5159=VERTEX_POINT('',#25369);
#5160=VERTEX_POINT('',#25371);
#5161=VERTEX_POINT('',#25377);
#5162=VERTEX_POINT('',#25381);
#5163=VERTEX_POINT('',#25383);
#5164=VERTEX_POINT('',#25387);
#5165=VERTEX_POINT('',#25389);
#5166=VERTEX_POINT('',#25393);
#5167=VERTEX_POINT('',#25395);
#5168=VERTEX_POINT('',#25399);
#5169=VERTEX_POINT('',#25401);
#5170=VERTEX_POINT('',#25405);
#5171=VERTEX_POINT('',#25407);
#5172=VERTEX_POINT('',#25411);
#5173=VERTEX_POINT('',#25413);
#5174=VERTEX_POINT('',#25417);
#5175=VERTEX_POINT('',#25419);
#5176=VERTEX_POINT('',#25423);
#5177=VERTEX_POINT('',#25425);
#5178=VERTEX_POINT('',#25429);
#5179=VERTEX_POINT('',#25431);
#5180=VERTEX_POINT('',#25435);
#5181=VERTEX_POINT('',#25437);
#5182=VERTEX_POINT('',#25441);
#5183=VERTEX_POINT('',#25443);
#5184=VERTEX_POINT('',#25445);
#5185=VERTEX_POINT('',#25447);
#5186=VERTEX_POINT('',#25450);
#5187=VERTEX_POINT('',#25452);
#5188=VERTEX_POINT('',#25454);
#5189=VERTEX_POINT('',#25456);
#5190=VERTEX_POINT('',#25459);
#5191=VERTEX_POINT('',#25461);
#5192=VERTEX_POINT('',#25463);
#5193=VERTEX_POINT('',#25465);
#5194=VERTEX_POINT('',#25468);
#5195=VERTEX_POINT('',#25470);
#5196=VERTEX_POINT('',#25472);
#5197=VERTEX_POINT('',#25474);
#5198=VERTEX_POINT('',#25477);
#5199=VERTEX_POINT('',#25479);
#5200=VERTEX_POINT('',#25481);
#5201=VERTEX_POINT('',#25483);
#5202=VERTEX_POINT('',#25486);
#5203=VERTEX_POINT('',#25488);
#5204=VERTEX_POINT('',#25490);
#5205=VERTEX_POINT('',#25492);
#5206=VERTEX_POINT('',#25495);
#5207=VERTEX_POINT('',#25497);
#5208=VERTEX_POINT('',#25499);
#5209=VERTEX_POINT('',#25501);
#5210=VERTEX_POINT('',#25504);
#5211=VERTEX_POINT('',#25506);
#5212=VERTEX_POINT('',#25508);
#5213=VERTEX_POINT('',#25510);
#5214=VERTEX_POINT('',#25513);
#5215=VERTEX_POINT('',#25515);
#5216=VERTEX_POINT('',#25517);
#5217=VERTEX_POINT('',#25519);
#5218=VERTEX_POINT('',#25522);
#5219=VERTEX_POINT('',#25524);
#5220=VERTEX_POINT('',#25526);
#5221=VERTEX_POINT('',#25528);
#5222=VERTEX_POINT('',#25531);
#5223=VERTEX_POINT('',#25533);
#5224=VERTEX_POINT('',#25537);
#5225=VERTEX_POINT('',#25539);
#5226=VERTEX_POINT('',#25545);
#5227=VERTEX_POINT('',#25547);
#5228=VERTEX_POINT('',#25552);
#5229=VERTEX_POINT('',#25556);
#5230=VERTEX_POINT('',#25566);
#5231=VERTEX_POINT('',#25568);
#5232=VERTEX_POINT('',#25573);
#5233=VERTEX_POINT('',#25577);
#5234=VERTEX_POINT('',#25586);
#5235=VERTEX_POINT('',#25588);
#5236=VERTEX_POINT('',#25593);
#5237=VERTEX_POINT('',#25597);
#5238=VERTEX_POINT('',#25606);
#5239=VERTEX_POINT('',#25608);
#5240=VERTEX_POINT('',#25613);
#5241=VERTEX_POINT('',#25617);
#5242=VERTEX_POINT('',#25626);
#5243=VERTEX_POINT('',#25628);
#5244=VERTEX_POINT('',#25633);
#5245=VERTEX_POINT('',#25637);
#5246=VERTEX_POINT('',#25646);
#5247=VERTEX_POINT('',#25648);
#5248=VERTEX_POINT('',#25653);
#5249=VERTEX_POINT('',#25657);
#5250=VERTEX_POINT('',#25666);
#5251=VERTEX_POINT('',#25668);
#5252=VERTEX_POINT('',#25673);
#5253=VERTEX_POINT('',#25677);
#5254=VERTEX_POINT('',#25686);
#5255=VERTEX_POINT('',#25688);
#5256=VERTEX_POINT('',#25693);
#5257=VERTEX_POINT('',#25697);
#5258=VERTEX_POINT('',#25706);
#5259=VERTEX_POINT('',#25708);
#5260=VERTEX_POINT('',#25713);
#5261=VERTEX_POINT('',#25717);
#5262=VERTEX_POINT('',#25726);
#5263=VERTEX_POINT('',#25728);
#5264=VERTEX_POINT('',#25733);
#5265=VERTEX_POINT('',#25737);
#5266=VERTEX_POINT('',#25772);
#5267=VERTEX_POINT('',#25774);
#5268=VERTEX_POINT('',#25776);
#5269=VERTEX_POINT('',#25780);
#5270=VERTEX_POINT('',#25781);
#5271=VERTEX_POINT('',#25784);
#5272=VERTEX_POINT('',#25788);
#5273=VERTEX_POINT('',#25790);
#5274=VERTEX_POINT('',#25794);
#5275=VERTEX_POINT('',#25798);
#5276=VERTEX_POINT('',#25800);
#5277=VERTEX_POINT('',#25804);
#5278=VERTEX_POINT('',#25808);
#5279=VERTEX_POINT('',#25810);
#5280=VERTEX_POINT('',#25814);
#5281=VERTEX_POINT('',#25818);
#5282=VERTEX_POINT('',#25820);
#5283=VERTEX_POINT('',#25824);
#5284=VERTEX_POINT('',#25828);
#5285=VERTEX_POINT('',#25830);
#5286=VERTEX_POINT('',#25834);
#5287=VERTEX_POINT('',#25838);
#5288=VERTEX_POINT('',#25840);
#5289=VERTEX_POINT('',#25844);
#5290=VERTEX_POINT('',#25848);
#5291=VERTEX_POINT('',#25850);
#5292=VERTEX_POINT('',#25859);
#5293=VERTEX_POINT('',#25860);
#5294=VERTEX_POINT('',#25862);
#5295=VERTEX_POINT('',#25864);
#5296=VERTEX_POINT('',#25868);
#5297=VERTEX_POINT('',#25870);
#5298=VERTEX_POINT('',#25874);
#5299=VERTEX_POINT('',#25876);
#5300=VERTEX_POINT('',#25880);
#5301=VERTEX_POINT('',#25882);
#5302=VERTEX_POINT('',#25886);
#5303=VERTEX_POINT('',#25888);
#5304=VERTEX_POINT('',#25892);
#5305=VERTEX_POINT('',#25894);
#5306=VERTEX_POINT('',#25898);
#5307=VERTEX_POINT('',#25900);
#5308=VERTEX_POINT('',#25904);
#5309=VERTEX_POINT('',#25906);
#5310=VERTEX_POINT('',#25910);
#5311=VERTEX_POINT('',#25912);
#5312=VERTEX_POINT('',#25916);
#5313=VERTEX_POINT('',#25918);
#5314=VERTEX_POINT('',#25922);
#5315=VERTEX_POINT('',#25924);
#5316=VERTEX_POINT('',#25933);
#5317=VERTEX_POINT('',#25934);
#5318=VERTEX_POINT('',#25936);
#5319=VERTEX_POINT('',#25938);
#5320=VERTEX_POINT('',#25940);
#5321=VERTEX_POINT('',#25942);
#5322=VERTEX_POINT('',#25944);
#5323=VERTEX_POINT('',#25946);
#5324=VERTEX_POINT('',#25948);
#5325=VERTEX_POINT('',#25950);
#5326=VERTEX_POINT('',#25952);
#5327=VERTEX_POINT('',#25954);
#5328=VERTEX_POINT('',#25958);
#5329=VERTEX_POINT('',#25960);
#5330=VERTEX_POINT('',#25964);
#5331=VERTEX_POINT('',#25968);
#5332=VERTEX_POINT('',#25972);
#5333=VERTEX_POINT('',#25976);
#5334=VERTEX_POINT('',#25980);
#5335=VERTEX_POINT('',#25984);
#5336=VERTEX_POINT('',#25988);
#5337=VERTEX_POINT('',#25992);
#5338=VERTEX_POINT('',#25996);
#5339=VERTEX_POINT('',#26000);
#5340=VERTEX_POINT('',#26007);
#5341=VERTEX_POINT('',#26008);
#5342=VERTEX_POINT('',#26010);
#5343=VERTEX_POINT('',#26012);
#5344=VERTEX_POINT('',#26014);
#5345=VERTEX_POINT('',#26016);
#5346=VERTEX_POINT('',#26018);
#5347=VERTEX_POINT('',#26020);
#5348=VERTEX_POINT('',#26022);
#5349=VERTEX_POINT('',#26024);
#5350=VERTEX_POINT('',#26026);
#5351=VERTEX_POINT('',#26028);
#5352=VERTEX_POINT('',#26032);
#5353=VERTEX_POINT('',#26034);
#5354=VERTEX_POINT('',#26038);
#5355=VERTEX_POINT('',#26042);
#5356=VERTEX_POINT('',#26046);
#5357=VERTEX_POINT('',#26050);
#5358=VERTEX_POINT('',#26054);
#5359=VERTEX_POINT('',#26058);
#5360=VERTEX_POINT('',#26062);
#5361=VERTEX_POINT('',#26066);
#5362=VERTEX_POINT('',#26070);
#5363=VERTEX_POINT('',#26074);
#5364=VERTEX_POINT('',#26081);
#5365=VERTEX_POINT('',#26082);
#5366=VERTEX_POINT('',#26084);
#5367=VERTEX_POINT('',#26086);
#5368=VERTEX_POINT('',#26090);
#5369=VERTEX_POINT('',#26092);
#5370=VERTEX_POINT('',#26096);
#5371=VERTEX_POINT('',#26098);
#5372=VERTEX_POINT('',#26102);
#5373=VERTEX_POINT('',#26104);
#5374=VERTEX_POINT('',#26108);
#5375=VERTEX_POINT('',#26110);
#5376=VERTEX_POINT('',#26114);
#5377=VERTEX_POINT('',#26116);
#5378=VERTEX_POINT('',#26120);
#5379=VERTEX_POINT('',#26122);
#5380=VERTEX_POINT('',#26126);
#5381=VERTEX_POINT('',#26128);
#5382=VERTEX_POINT('',#26132);
#5383=VERTEX_POINT('',#26134);
#5384=VERTEX_POINT('',#26138);
#5385=VERTEX_POINT('',#26140);
#5386=VERTEX_POINT('',#26144);
#5387=VERTEX_POINT('',#26146);
#5388=VERTEX_POINT('',#26155);
#5389=VERTEX_POINT('',#26156);
#5390=VERTEX_POINT('',#26158);
#5391=VERTEX_POINT('',#26160);
#5392=VERTEX_POINT('',#26164);
#5393=VERTEX_POINT('',#26166);
#5394=VERTEX_POINT('',#26170);
#5395=VERTEX_POINT('',#26172);
#5396=VERTEX_POINT('',#26176);
#5397=VERTEX_POINT('',#26178);
#5398=VERTEX_POINT('',#26182);
#5399=VERTEX_POINT('',#26184);
#5400=VERTEX_POINT('',#26188);
#5401=VERTEX_POINT('',#26190);
#5402=VERTEX_POINT('',#26194);
#5403=VERTEX_POINT('',#26196);
#5404=VERTEX_POINT('',#26200);
#5405=VERTEX_POINT('',#26202);
#5406=VERTEX_POINT('',#26206);
#5407=VERTEX_POINT('',#26208);
#5408=VERTEX_POINT('',#26212);
#5409=VERTEX_POINT('',#26214);
#5410=VERTEX_POINT('',#26218);
#5411=VERTEX_POINT('',#26220);
#5412=VERTEX_POINT('',#26229);
#5413=VERTEX_POINT('',#26230);
#5414=VERTEX_POINT('',#26232);
#5415=VERTEX_POINT('',#26234);
#5416=VERTEX_POINT('',#26236);
#5417=VERTEX_POINT('',#26238);
#5418=VERTEX_POINT('',#26240);
#5419=VERTEX_POINT('',#26242);
#5420=VERTEX_POINT('',#26244);
#5421=VERTEX_POINT('',#26246);
#5422=VERTEX_POINT('',#26248);
#5423=VERTEX_POINT('',#26250);
#5424=VERTEX_POINT('',#26254);
#5425=VERTEX_POINT('',#26256);
#5426=VERTEX_POINT('',#26260);
#5427=VERTEX_POINT('',#26264);
#5428=VERTEX_POINT('',#26268);
#5429=VERTEX_POINT('',#26272);
#5430=VERTEX_POINT('',#26276);
#5431=VERTEX_POINT('',#26280);
#5432=VERTEX_POINT('',#26284);
#5433=VERTEX_POINT('',#26288);
#5434=VERTEX_POINT('',#26292);
#5435=VERTEX_POINT('',#26296);
#5436=VERTEX_POINT('',#26303);
#5437=VERTEX_POINT('',#26304);
#5438=VERTEX_POINT('',#26306);
#5439=VERTEX_POINT('',#26308);
#5440=VERTEX_POINT('',#26312);
#5441=VERTEX_POINT('',#26314);
#5442=VERTEX_POINT('',#26318);
#5443=VERTEX_POINT('',#26320);
#5444=VERTEX_POINT('',#26324);
#5445=VERTEX_POINT('',#26326);
#5446=VERTEX_POINT('',#26330);
#5447=VERTEX_POINT('',#26332);
#5448=VERTEX_POINT('',#26336);
#5449=VERTEX_POINT('',#26338);
#5450=VERTEX_POINT('',#26342);
#5451=VERTEX_POINT('',#26344);
#5452=VERTEX_POINT('',#26348);
#5453=VERTEX_POINT('',#26350);
#5454=VERTEX_POINT('',#26354);
#5455=VERTEX_POINT('',#26356);
#5456=VERTEX_POINT('',#26360);
#5457=VERTEX_POINT('',#26362);
#5458=VERTEX_POINT('',#26366);
#5459=VERTEX_POINT('',#26368);
#5460=VERTEX_POINT('',#26377);
#5461=VERTEX_POINT('',#26378);
#5462=VERTEX_POINT('',#26380);
#5463=VERTEX_POINT('',#26382);
#5464=VERTEX_POINT('',#26384);
#5465=VERTEX_POINT('',#26386);
#5466=VERTEX_POINT('',#26388);
#5467=VERTEX_POINT('',#26390);
#5468=VERTEX_POINT('',#26392);
#5469=VERTEX_POINT('',#26394);
#5470=VERTEX_POINT('',#26396);
#5471=VERTEX_POINT('',#26398);
#5472=VERTEX_POINT('',#26402);
#5473=VERTEX_POINT('',#26404);
#5474=VERTEX_POINT('',#26408);
#5475=VERTEX_POINT('',#26412);
#5476=VERTEX_POINT('',#26416);
#5477=VERTEX_POINT('',#26420);
#5478=VERTEX_POINT('',#26424);
#5479=VERTEX_POINT('',#26428);
#5480=VERTEX_POINT('',#26432);
#5481=VERTEX_POINT('',#26436);
#5482=VERTEX_POINT('',#26440);
#5483=VERTEX_POINT('',#26444);
#5484=VERTEX_POINT('',#26451);
#5485=VERTEX_POINT('',#26452);
#5486=VERTEX_POINT('',#26454);
#5487=VERTEX_POINT('',#26456);
#5488=VERTEX_POINT('',#26458);
#5489=VERTEX_POINT('',#26460);
#5490=VERTEX_POINT('',#26462);
#5491=VERTEX_POINT('',#26464);
#5492=VERTEX_POINT('',#26466);
#5493=VERTEX_POINT('',#26468);
#5494=VERTEX_POINT('',#26470);
#5495=VERTEX_POINT('',#26472);
#5496=VERTEX_POINT('',#26476);
#5497=VERTEX_POINT('',#26478);
#5498=VERTEX_POINT('',#26482);
#5499=VERTEX_POINT('',#26486);
#5500=VERTEX_POINT('',#26490);
#5501=VERTEX_POINT('',#26494);
#5502=VERTEX_POINT('',#26498);
#5503=VERTEX_POINT('',#26502);
#5504=VERTEX_POINT('',#26506);
#5505=VERTEX_POINT('',#26510);
#5506=VERTEX_POINT('',#26514);
#5507=VERTEX_POINT('',#26518);
#5508=VERTEX_POINT('',#26525);
#5509=VERTEX_POINT('',#26526);
#5510=VERTEX_POINT('',#26528);
#5511=VERTEX_POINT('',#26530);
#5512=VERTEX_POINT('',#26532);
#5513=VERTEX_POINT('',#26534);
#5514=VERTEX_POINT('',#26536);
#5515=VERTEX_POINT('',#26538);
#5516=VERTEX_POINT('',#26540);
#5517=VERTEX_POINT('',#26542);
#5518=VERTEX_POINT('',#26544);
#5519=VERTEX_POINT('',#26546);
#5520=VERTEX_POINT('',#26550);
#5521=VERTEX_POINT('',#26552);
#5522=VERTEX_POINT('',#26556);
#5523=VERTEX_POINT('',#26560);
#5524=VERTEX_POINT('',#26564);
#5525=VERTEX_POINT('',#26568);
#5526=VERTEX_POINT('',#26572);
#5527=VERTEX_POINT('',#26576);
#5528=VERTEX_POINT('',#26580);
#5529=VERTEX_POINT('',#26584);
#5530=VERTEX_POINT('',#26588);
#5531=VERTEX_POINT('',#26592);
#5532=VERTEX_POINT('',#26599);
#5533=VERTEX_POINT('',#26600);
#5534=VERTEX_POINT('',#26602);
#5535=VERTEX_POINT('',#26604);
#5536=VERTEX_POINT('',#26608);
#5537=VERTEX_POINT('',#26610);
#5538=VERTEX_POINT('',#26614);
#5539=VERTEX_POINT('',#26616);
#5540=VERTEX_POINT('',#26620);
#5541=VERTEX_POINT('',#26622);
#5542=VERTEX_POINT('',#26626);
#5543=VERTEX_POINT('',#26628);
#5544=VERTEX_POINT('',#26632);
#5545=VERTEX_POINT('',#26634);
#5546=VERTEX_POINT('',#26638);
#5547=VERTEX_POINT('',#26640);
#5548=VERTEX_POINT('',#26644);
#5549=VERTEX_POINT('',#26646);
#5550=VERTEX_POINT('',#26655);
#5551=VERTEX_POINT('',#26656);
#5552=VERTEX_POINT('',#26658);
#5553=VERTEX_POINT('',#26660);
#5554=VERTEX_POINT('',#26664);
#5555=VERTEX_POINT('',#26666);
#5556=VERTEX_POINT('',#26670);
#5557=VERTEX_POINT('',#26672);
#5558=VERTEX_POINT('',#26676);
#5559=VERTEX_POINT('',#26678);
#5560=VERTEX_POINT('',#26682);
#5561=VERTEX_POINT('',#26684);
#5562=VERTEX_POINT('',#26688);
#5563=VERTEX_POINT('',#26690);
#5564=VERTEX_POINT('',#26694);
#5565=VERTEX_POINT('',#26696);
#5566=VERTEX_POINT('',#26700);
#5567=VERTEX_POINT('',#26702);
#5568=VERTEX_POINT('',#26711);
#5569=VERTEX_POINT('',#26712);
#5570=VERTEX_POINT('',#26714);
#5571=VERTEX_POINT('',#26716);
#5572=VERTEX_POINT('',#26720);
#5573=VERTEX_POINT('',#26722);
#5574=VERTEX_POINT('',#26726);
#5575=VERTEX_POINT('',#26728);
#5576=VERTEX_POINT('',#26732);
#5577=VERTEX_POINT('',#26734);
#5578=VERTEX_POINT('',#26738);
#5579=VERTEX_POINT('',#26740);
#5580=VERTEX_POINT('',#26744);
#5581=VERTEX_POINT('',#26746);
#5582=VERTEX_POINT('',#26750);
#5583=VERTEX_POINT('',#26752);
#5584=VERTEX_POINT('',#26756);
#5585=VERTEX_POINT('',#26758);
#5586=VERTEX_POINT('',#26767);
#5587=VERTEX_POINT('',#26768);
#5588=VERTEX_POINT('',#26770);
#5589=VERTEX_POINT('',#26772);
#5590=VERTEX_POINT('',#26776);
#5591=VERTEX_POINT('',#26778);
#5592=VERTEX_POINT('',#26782);
#5593=VERTEX_POINT('',#26784);
#5594=VERTEX_POINT('',#26788);
#5595=VERTEX_POINT('',#26790);
#5596=VERTEX_POINT('',#26794);
#5597=VERTEX_POINT('',#26796);
#5598=VERTEX_POINT('',#26800);
#5599=VERTEX_POINT('',#26802);
#5600=VERTEX_POINT('',#26806);
#5601=VERTEX_POINT('',#26808);
#5602=VERTEX_POINT('',#26812);
#5603=VERTEX_POINT('',#26814);
#5604=VERTEX_POINT('',#26823);
#5605=VERTEX_POINT('',#26824);
#5606=VERTEX_POINT('',#26826);
#5607=VERTEX_POINT('',#26828);
#5608=VERTEX_POINT('',#26830);
#5609=VERTEX_POINT('',#26832);
#5610=VERTEX_POINT('',#26834);
#5611=VERTEX_POINT('',#26836);
#5612=VERTEX_POINT('',#26838);
#5613=VERTEX_POINT('',#26842);
#5614=VERTEX_POINT('',#26844);
#5615=VERTEX_POINT('',#26848);
#5616=VERTEX_POINT('',#26852);
#5617=VERTEX_POINT('',#26856);
#5618=VERTEX_POINT('',#26860);
#5619=VERTEX_POINT('',#26864);
#5620=VERTEX_POINT('',#26868);
#5621=VERTEX_POINT('',#26872);
#5622=VERTEX_POINT('',#26879);
#5623=VERTEX_POINT('',#26880);
#5624=VERTEX_POINT('',#26882);
#5625=VERTEX_POINT('',#26884);
#5626=VERTEX_POINT('',#26888);
#5627=VERTEX_POINT('',#26890);
#5628=VERTEX_POINT('',#26894);
#5629=VERTEX_POINT('',#26896);
#5630=VERTEX_POINT('',#26900);
#5631=VERTEX_POINT('',#26902);
#5632=VERTEX_POINT('',#26906);
#5633=VERTEX_POINT('',#26908);
#5634=VERTEX_POINT('',#26912);
#5635=VERTEX_POINT('',#26914);
#5636=VERTEX_POINT('',#26918);
#5637=VERTEX_POINT('',#26920);
#5638=VERTEX_POINT('',#26924);
#5639=VERTEX_POINT('',#26926);
#5640=VERTEX_POINT('',#26935);
#5641=VERTEX_POINT('',#26936);
#5642=VERTEX_POINT('',#26938);
#5643=VERTEX_POINT('',#26940);
#5644=VERTEX_POINT('',#26942);
#5645=VERTEX_POINT('',#26944);
#5646=VERTEX_POINT('',#26946);
#5647=VERTEX_POINT('',#26948);
#5648=VERTEX_POINT('',#26950);
#5649=VERTEX_POINT('',#26954);
#5650=VERTEX_POINT('',#26956);
#5651=VERTEX_POINT('',#26960);
#5652=VERTEX_POINT('',#26964);
#5653=VERTEX_POINT('',#26968);
#5654=VERTEX_POINT('',#26972);
#5655=VERTEX_POINT('',#26976);
#5656=VERTEX_POINT('',#26980);
#5657=VERTEX_POINT('',#26984);
#5658=VERTEX_POINT('',#26991);
#5659=VERTEX_POINT('',#26992);
#5660=VERTEX_POINT('',#26994);
#5661=VERTEX_POINT('',#26996);
#5662=VERTEX_POINT('',#26998);
#5663=VERTEX_POINT('',#27000);
#5664=VERTEX_POINT('',#27002);
#5665=VERTEX_POINT('',#27004);
#5666=VERTEX_POINT('',#27006);
#5667=VERTEX_POINT('',#27010);
#5668=VERTEX_POINT('',#27012);
#5669=VERTEX_POINT('',#27016);
#5670=VERTEX_POINT('',#27020);
#5671=VERTEX_POINT('',#27024);
#5672=VERTEX_POINT('',#27028);
#5673=VERTEX_POINT('',#27032);
#5674=VERTEX_POINT('',#27036);
#5675=VERTEX_POINT('',#27040);
#5676=VERTEX_POINT('',#27047);
#5677=VERTEX_POINT('',#27048);
#5678=VERTEX_POINT('',#27050);
#5679=VERTEX_POINT('',#27052);
#5680=VERTEX_POINT('',#27056);
#5681=VERTEX_POINT('',#27058);
#5682=VERTEX_POINT('',#27062);
#5683=VERTEX_POINT('',#27064);
#5684=VERTEX_POINT('',#27068);
#5685=VERTEX_POINT('',#27070);
#5686=VERTEX_POINT('',#27074);
#5687=VERTEX_POINT('',#27076);
#5688=VERTEX_POINT('',#27080);
#5689=VERTEX_POINT('',#27082);
#5690=VERTEX_POINT('',#27086);
#5691=VERTEX_POINT('',#27088);
#5692=VERTEX_POINT('',#27092);
#5693=VERTEX_POINT('',#27094);
#5694=VERTEX_POINT('',#27103);
#5695=VERTEX_POINT('',#27104);
#5696=VERTEX_POINT('',#27106);
#5697=VERTEX_POINT('',#27108);
#5698=VERTEX_POINT('',#27110);
#5699=VERTEX_POINT('',#27112);
#5700=VERTEX_POINT('',#27114);
#5701=VERTEX_POINT('',#27116);
#5702=VERTEX_POINT('',#27118);
#5703=VERTEX_POINT('',#27122);
#5704=VERTEX_POINT('',#27124);
#5705=VERTEX_POINT('',#27128);
#5706=VERTEX_POINT('',#27132);
#5707=VERTEX_POINT('',#27136);
#5708=VERTEX_POINT('',#27140);
#5709=VERTEX_POINT('',#27144);
#5710=VERTEX_POINT('',#27148);
#5711=VERTEX_POINT('',#27152);
#5712=VERTEX_POINT('',#27159);
#5713=VERTEX_POINT('',#27160);
#5714=VERTEX_POINT('',#27162);
#5715=VERTEX_POINT('',#27164);
#5716=VERTEX_POINT('',#27168);
#5717=VERTEX_POINT('',#27169);
#5718=VERTEX_POINT('',#27171);
#5719=VERTEX_POINT('',#27173);
#5720=VERTEX_POINT('',#27177);
#5721=VERTEX_POINT('',#27178);
#5722=VERTEX_POINT('',#27180);
#5723=VERTEX_POINT('',#27182);
#5724=VERTEX_POINT('',#27186);
#5725=VERTEX_POINT('',#27187);
#5726=VERTEX_POINT('',#27189);
#5727=VERTEX_POINT('',#27191);
#5728=VERTEX_POINT('',#27195);
#5729=VERTEX_POINT('',#27196);
#5730=VERTEX_POINT('',#27198);
#5731=VERTEX_POINT('',#27200);
#5732=VERTEX_POINT('',#27204);
#5733=VERTEX_POINT('',#27205);
#5734=VERTEX_POINT('',#27207);
#5735=VERTEX_POINT('',#27209);
#5736=VERTEX_POINT('',#27213);
#5737=VERTEX_POINT('',#27214);
#5738=VERTEX_POINT('',#27216);
#5739=VERTEX_POINT('',#27218);
#5740=VERTEX_POINT('',#27222);
#5741=VERTEX_POINT('',#27223);
#5742=VERTEX_POINT('',#27225);
#5743=VERTEX_POINT('',#27227);
#5744=VERTEX_POINT('',#27235);
#5745=VERTEX_POINT('',#27237);
#5746=VERTEX_POINT('',#27240);
#5747=VERTEX_POINT('',#27242);
#5748=VERTEX_POINT('',#27245);
#5749=VERTEX_POINT('',#27247);
#5750=VERTEX_POINT('',#27250);
#5751=VERTEX_POINT('',#27252);
#5752=VERTEX_POINT('',#27260);
#5753=VERTEX_POINT('',#27262);
#5754=VERTEX_POINT('',#27265);
#5755=VERTEX_POINT('',#27267);
#5756=VERTEX_POINT('',#27270);
#5757=VERTEX_POINT('',#27272);
#5758=VERTEX_POINT('',#27275);
#5759=VERTEX_POINT('',#27277);
#5760=VERTEX_POINT('',#27305);
#5761=VERTEX_POINT('',#27307);
#5762=VERTEX_POINT('',#27311);
#5763=VERTEX_POINT('',#27313);
#5764=VERTEX_POINT('',#27317);
#5765=VERTEX_POINT('',#27318);
#5766=VERTEX_POINT('',#27320);
#5767=VERTEX_POINT('',#27322);
#5768=VERTEX_POINT('',#27326);
#5769=VERTEX_POINT('',#27328);
#5770=VERTEX_POINT('',#27332);
#5771=VERTEX_POINT('',#27334);
#5772=VERTEX_POINT('',#27338);
#5773=VERTEX_POINT('',#27340);
#5774=VERTEX_POINT('',#27344);
#5775=VERTEX_POINT('',#27346);
#5776=VERTEX_POINT('',#27350);
#5777=VERTEX_POINT('',#27352);
#5778=VERTEX_POINT('',#27356);
#5779=VERTEX_POINT('',#27358);
#5780=VERTEX_POINT('',#27362);
#5781=VERTEX_POINT('',#27364);
#5782=VERTEX_POINT('',#27368);
#5783=VERTEX_POINT('',#27370);
#5784=VERTEX_POINT('',#27374);
#5785=VERTEX_POINT('',#27376);
#5786=VERTEX_POINT('',#27380);
#5787=VERTEX_POINT('',#27382);
#5788=VERTEX_POINT('',#27391);
#5789=VERTEX_POINT('',#27393);
#5790=VERTEX_POINT('',#27397);
#5791=VERTEX_POINT('',#27399);
#5792=VERTEX_POINT('',#27403);
#5793=VERTEX_POINT('',#27404);
#5794=VERTEX_POINT('',#27406);
#5795=VERTEX_POINT('',#27408);
#5796=VERTEX_POINT('',#27412);
#5797=VERTEX_POINT('',#27414);
#5798=VERTEX_POINT('',#27418);
#5799=VERTEX_POINT('',#27420);
#5800=VERTEX_POINT('',#27424);
#5801=VERTEX_POINT('',#27426);
#5802=VERTEX_POINT('',#27430);
#5803=VERTEX_POINT('',#27432);
#5804=VERTEX_POINT('',#27436);
#5805=VERTEX_POINT('',#27438);
#5806=VERTEX_POINT('',#27442);
#5807=VERTEX_POINT('',#27444);
#5808=VERTEX_POINT('',#27448);
#5809=VERTEX_POINT('',#27450);
#5810=VERTEX_POINT('',#27459);
#5811=VERTEX_POINT('',#27461);
#5812=VERTEX_POINT('',#27465);
#5813=VERTEX_POINT('',#27467);
#5814=VERTEX_POINT('',#27471);
#5815=VERTEX_POINT('',#27472);
#5816=VERTEX_POINT('',#27474);
#5817=VERTEX_POINT('',#27476);
#5818=VERTEX_POINT('',#27480);
#5819=VERTEX_POINT('',#27482);
#5820=VERTEX_POINT('',#27486);
#5821=VERTEX_POINT('',#27488);
#5822=VERTEX_POINT('',#27492);
#5823=VERTEX_POINT('',#27494);
#5824=VERTEX_POINT('',#27498);
#5825=VERTEX_POINT('',#27500);
#5826=VERTEX_POINT('',#27504);
#5827=VERTEX_POINT('',#27506);
#5828=VERTEX_POINT('',#27510);
#5829=VERTEX_POINT('',#27512);
#5830=VERTEX_POINT('',#27516);
#5831=VERTEX_POINT('',#27518);
#5832=EDGE_CURVE('',#4768,#4769,#2744,.T.);
#5833=EDGE_CURVE('',#4770,#4768,#2688,.T.);
#5834=EDGE_CURVE('',#4769,#4770,#2140,.T.);
#5835=EDGE_CURVE('',#4771,#4772,#2141,.T.);
#5836=EDGE_CURVE('',#4772,#4771,#2142,.T.);
#5837=EDGE_CURVE('',#4772,#4773,#2143,.T.);
#5838=EDGE_CURVE('',#4773,#4773,#2144,.T.);
#5839=EDGE_CURVE('',#4774,#4775,#2145,.T.);
#5840=EDGE_CURVE('',#4776,#4774,#2745,.T.);
#5841=EDGE_CURVE('',#4776,#4777,#2146,.T.);
#5842=EDGE_CURVE('',#4775,#4777,#2746,.T.);
#5843=EDGE_CURVE('',#4778,#4779,#2147,.T.);
#5844=EDGE_CURVE('',#4779,#4780,#2148,.T.);
#5845=EDGE_CURVE('',#4781,#4780,#2747,.T.);
#5846=EDGE_CURVE('',#4782,#4781,#2149,.T.);
#5847=EDGE_CURVE('',#4778,#4782,#2748,.T.);
#5848=EDGE_CURVE('',#4783,#4784,#2150,.T.);
#5849=EDGE_CURVE('',#4785,#4783,#2749,.T.);
#5850=EDGE_CURVE('',#4785,#4786,#2151,.T.);
#5851=EDGE_CURVE('',#4784,#4786,#2750,.T.);
#5852=EDGE_CURVE('',#4787,#4788,#2152,.T.);
#5853=EDGE_CURVE('',#4787,#4789,#2153,.T.);
#5854=EDGE_CURVE('',#4789,#4788,#2154,.T.);
#5855=EDGE_CURVE('',#4790,#4791,#2155,.T.);
#5856=EDGE_CURVE('',#4791,#4792,#2156,.T.);
#5857=EDGE_CURVE('',#4790,#4792,#2157,.T.);
#5858=EDGE_CURVE('',#4793,#4794,#2158,.T.);
#5859=EDGE_CURVE('',#4794,#4795,#2159,.T.);
#5860=EDGE_CURVE('',#4793,#4795,#2160,.T.);
#5861=EDGE_CURVE('',#4796,#4797,#2161,.T.);
#5862=EDGE_CURVE('',#4796,#4798,#2162,.T.);
#5863=EDGE_CURVE('',#4798,#4797,#2163,.T.);
#5864=EDGE_CURVE('',#4799,#4799,#2164,.T.);
#5865=EDGE_CURVE('',#4799,#4800,#2165,.T.);
#5866=EDGE_CURVE('',#4801,#4800,#2166,.T.);
#5867=EDGE_CURVE('',#4800,#4801,#2167,.T.);
#5868=EDGE_CURVE('',#4802,#4803,#2168,.T.);
#5869=EDGE_CURVE('',#4803,#4802,#2169,.T.);
#5870=EDGE_CURVE('',#4803,#4804,#2170,.T.);
#5871=EDGE_CURVE('',#4804,#4804,#2171,.T.);
#5872=EDGE_CURVE('',#4805,#4805,#2172,.T.);
#5873=EDGE_CURVE('',#4805,#4806,#2751,.T.);
#5874=EDGE_CURVE('',#4806,#4806,#2173,.T.);
#5875=EDGE_CURVE('',#4807,#4807,#2174,.T.);
#5876=EDGE_CURVE('',#4807,#4805,#2752,.T.);
#5877=EDGE_CURVE('',#4808,#4808,#2175,.T.);
#5878=EDGE_CURVE('',#4808,#4809,#2753,.T.);
#5879=EDGE_CURVE('',#4809,#4809,#2176,.T.);
#5880=EDGE_CURVE('',#4810,#4810,#2177,.T.);
#5881=EDGE_CURVE('',#4810,#4808,#2754,.T.);
#5882=EDGE_CURVE('',#4811,#4811,#2178,.T.);
#5883=EDGE_CURVE('',#4811,#4812,#2755,.T.);
#5884=EDGE_CURVE('',#4812,#4812,#2179,.T.);
#5885=EDGE_CURVE('',#4813,#4813,#2180,.T.);
#5886=EDGE_CURVE('',#4813,#4811,#2756,.T.);
#5887=EDGE_CURVE('',#4814,#4814,#2181,.T.);
#5888=EDGE_CURVE('',#4814,#4815,#2757,.T.);
#5889=EDGE_CURVE('',#4815,#4815,#2182,.T.);
#5890=EDGE_CURVE('',#4816,#4816,#2183,.T.);
#5891=EDGE_CURVE('',#4816,#4814,#2758,.T.);
#5892=EDGE_CURVE('',#4817,#4817,#2184,.T.);
#5893=EDGE_CURVE('',#4817,#4818,#2759,.T.);
#5894=EDGE_CURVE('',#4818,#4818,#2185,.T.);
#5895=EDGE_CURVE('',#4819,#4819,#2186,.T.);
#5896=EDGE_CURVE('',#4819,#4817,#2760,.T.);
#5897=EDGE_CURVE('',#4820,#4820,#2187,.T.);
#5898=EDGE_CURVE('',#4820,#4821,#2761,.T.);
#5899=EDGE_CURVE('',#4821,#4821,#2188,.T.);
#5900=EDGE_CURVE('',#4822,#4822,#2189,.T.);
#5901=EDGE_CURVE('',#4822,#4820,#2762,.T.);
#5902=EDGE_CURVE('',#4802,#4801,#2763,.T.);
#5903=EDGE_CURVE('',#4823,#4823,#2190,.T.);
#5904=EDGE_CURVE('',#4823,#4824,#2764,.T.);
#5905=EDGE_CURVE('',#4824,#4824,#2191,.T.);
#5906=EDGE_CURVE('',#4825,#4826,#2192,.T.);
#5907=EDGE_CURVE('',#4826,#4825,#2193,.T.);
#5908=EDGE_CURVE('',#4826,#4827,#2765,.T.);
#5909=EDGE_CURVE('',#4827,#4827,#2194,.T.);
#5910=EDGE_CURVE('',#4825,#4823,#2766,.T.);
#5911=EDGE_CURVE('',#4828,#4828,#2195,.T.);
#5912=EDGE_CURVE('',#4828,#4829,#2767,.T.);
#5913=EDGE_CURVE('',#4829,#4829,#2196,.T.);
#5914=EDGE_CURVE('',#4830,#4830,#2197,.T.);
#5915=EDGE_CURVE('',#4830,#4831,#2768,.T.);
#5916=EDGE_CURVE('',#4831,#4831,#2198,.T.);
#5917=EDGE_CURVE('',#4832,#4832,#2199,.T.);
#5918=EDGE_CURVE('',#4832,#4833,#2769,.T.);
#5919=EDGE_CURVE('',#4833,#4833,#2200,.T.);
#5920=EDGE_CURVE('',#4834,#4834,#2201,.T.);
#5921=EDGE_CURVE('',#4834,#4835,#2770,.T.);
#5922=EDGE_CURVE('',#4835,#4835,#2202,.T.);
#5923=EDGE_CURVE('',#4836,#4837,#2203,.T.);
#5924=EDGE_CURVE('',#4837,#4838,#2771,.T.);
#5925=EDGE_CURVE('',#4839,#4838,#2204,.T.);
#5926=EDGE_CURVE('',#4839,#4836,#2772,.T.);
#5927=EDGE_CURVE('',#4840,#4769,#2205,.T.);
#5928=EDGE_CURVE('',#4836,#4840,#2689,.T.);
#5929=EDGE_CURVE('',#4841,#4839,#2690,.T.);
#5930=EDGE_CURVE('',#4842,#4841,#2206,.T.);
#5931=EDGE_CURVE('',#4843,#4842,#2691,.T.);
#5932=EDGE_CURVE('',#4844,#4843,#2773,.T.);
#5933=EDGE_CURVE('',#4844,#4844,#2207,.T.);
#5934=EDGE_CURVE('',#4843,#4768,#2774,.T.);
#5935=EDGE_CURVE('',#4845,#4846,#2208,.T.);
#5936=EDGE_CURVE('',#4847,#4845,#2209,.T.);
#5937=EDGE_CURVE('',#4848,#4847,#2775,.T.);
#5938=EDGE_CURVE('',#4848,#4849,#2210,.T.);
#5939=EDGE_CURVE('',#4849,#4850,#2211,.T.);
#5940=EDGE_CURVE('',#4846,#4850,#2776,.T.);
#5941=EDGE_CURVE('',#4771,#4851,#2777,.T.);
#5942=EDGE_CURVE('',#4852,#4851,#2778,.T.);
#5943=EDGE_CURVE('',#4852,#4853,#2779,.T.);
#5944=EDGE_CURVE('',#4853,#4853,#2212,.T.);
#5945=EDGE_CURVE('',#4852,#4854,#2692,.T.);
#5946=EDGE_CURVE('',#4854,#4855,#2213,.T.);
#5947=EDGE_CURVE('',#4855,#4848,#2693,.T.);
#5948=EDGE_CURVE('',#4847,#4856,#2694,.T.);
#5949=EDGE_CURVE('',#4856,#4857,#2214,.T.);
#5950=EDGE_CURVE('',#4857,#4851,#2695,.T.);
#5951=EDGE_CURVE('',#4777,#4858,#2215,.T.);
#5952=EDGE_CURVE('',#4858,#4859,#2696,.T.);
#5953=EDGE_CURVE('',#4859,#4860,#2780,.T.);
#5954=EDGE_CURVE('',#4860,#4861,#2697,.T.);
#5955=EDGE_CURVE('',#4861,#4784,#2216,.T.);
#5956=EDGE_CURVE('',#4862,#4786,#2698,.T.);
#5957=EDGE_CURVE('',#4862,#4863,#2217,.T.);
#5958=EDGE_CURVE('',#4863,#4864,#2699,.T.);
#5959=EDGE_CURVE('',#4864,#4865,#2781,.T.);
#5960=EDGE_CURVE('',#4865,#4866,#2700,.T.);
#5961=EDGE_CURVE('',#4866,#4867,#2218,.T.);
#5962=EDGE_CURVE('',#4778,#4867,#2701,.T.);
#5963=EDGE_CURVE('',#4782,#4868,#2219,.T.);
#5964=EDGE_CURVE('',#4868,#4869,#2702,.T.);
#5965=EDGE_CURVE('',#4869,#4870,#2782,.T.);
#5966=EDGE_CURVE('',#4870,#4871,#2703,.T.);
#5967=EDGE_CURVE('',#4871,#4775,#2220,.T.);
#5968=EDGE_CURVE('',#4797,#4872,#2221,.T.);
#5969=EDGE_CURVE('',#4872,#4873,#2704,.T.);
#5970=EDGE_CURVE('',#4873,#4874,#2783,.T.);
#5971=EDGE_CURVE('',#4874,#4875,#2705,.T.);
#5972=EDGE_CURVE('',#4875,#4793,#2222,.T.);
#5973=EDGE_CURVE('',#4793,#4790,#2784,.T.);
#5974=EDGE_CURVE('',#4790,#4876,#2223,.T.);
#5975=EDGE_CURVE('',#4876,#4877,#2706,.T.);
#5976=EDGE_CURVE('',#4877,#4878,#2785,.T.);
#5977=EDGE_CURVE('',#4878,#4879,#2707,.T.);
#5978=EDGE_CURVE('',#4879,#4788,#2224,.T.);
#5979=EDGE_CURVE('',#4788,#4880,#2786,.T.);
#5980=EDGE_CURVE('',#4881,#4880,#2708,.T.);
#5981=EDGE_CURVE('',#4881,#4882,#2225,.T.);
#5982=EDGE_CURVE('',#4882,#4883,#2709,.T.);
#5983=EDGE_CURVE('',#4883,#4884,#2787,.T.);
#5984=EDGE_CURVE('',#4884,#4885,#2710,.T.);
#5985=EDGE_CURVE('',#4885,#4886,#2226,.T.);
#5986=EDGE_CURVE('',#4887,#4886,#2711,.T.);
#5987=EDGE_CURVE('',#4887,#4797,#2788,.T.);
#5988=EDGE_CURVE('',#4888,#4889,#2789,.T.);
#5989=EDGE_CURVE('',#4889,#4890,#2790,.T.);
#5990=EDGE_CURVE('',#4890,#4891,#2791,.T.);
#5991=EDGE_CURVE('',#4891,#4892,#2792,.T.);
#5992=EDGE_CURVE('',#4892,#4893,#2793,.T.);
#5993=EDGE_CURVE('',#4893,#4888,#2794,.T.);
#5994=EDGE_CURVE('',#4894,#4895,#2795,.T.);
#5995=EDGE_CURVE('',#4895,#4896,#2796,.T.);
#5996=EDGE_CURVE('',#4896,#4897,#2797,.T.);
#5997=EDGE_CURVE('',#4897,#4898,#2798,.T.);
#5998=EDGE_CURVE('',#4898,#4789,#2799,.T.);
#5999=EDGE_CURVE('',#4789,#4899,#2800,.T.);
#6000=EDGE_CURVE('',#4900,#4899,#2227,.T.);
#6001=EDGE_CURVE('',#4900,#4901,#2801,.T.);
#6002=EDGE_CURVE('',#4902,#4901,#2228,.T.);
#6003=EDGE_CURVE('',#4902,#4791,#2802,.T.);
#6004=EDGE_CURVE('',#4791,#4795,#2803,.T.);
#6005=EDGE_CURVE('',#4795,#4903,#2804,.T.);
#6006=EDGE_CURVE('',#4904,#4903,#2229,.T.);
#6007=EDGE_CURVE('',#4904,#4905,#2805,.T.);
#6008=EDGE_CURVE('',#4906,#4905,#2230,.T.);
#6009=EDGE_CURVE('',#4906,#4796,#2806,.T.);
#6010=EDGE_CURVE('',#4796,#4907,#2807,.T.);
#6011=EDGE_CURVE('',#4907,#4894,#2808,.T.);
#6012=EDGE_CURVE('',#4908,#4781,#2809,.T.);
#6013=EDGE_CURVE('',#4780,#4909,#2810,.T.);
#6014=EDGE_CURVE('',#4909,#4910,#2811,.T.);
#6015=EDGE_CURVE('',#4910,#4911,#2812,.T.);
#6016=EDGE_CURVE('',#4911,#4912,#2813,.T.);
#6017=EDGE_CURVE('',#4912,#4785,#2814,.T.);
#6018=EDGE_CURVE('',#4783,#4913,#2815,.T.);
#6019=EDGE_CURVE('',#4914,#4913,#2231,.T.);
#6020=EDGE_CURVE('',#4914,#4915,#2816,.T.);
#6021=EDGE_CURVE('',#4916,#4915,#2232,.T.);
#6022=EDGE_CURVE('',#4916,#4776,#2817,.T.);
#6023=EDGE_CURVE('',#4774,#4917,#2818,.T.);
#6024=EDGE_CURVE('',#4918,#4917,#2233,.T.);
#6025=EDGE_CURVE('',#4918,#4919,#2819,.T.);
#6026=EDGE_CURVE('',#4908,#4919,#2234,.T.);
#6027=EDGE_CURVE('',#4920,#4846,#2235,.T.);
#6028=EDGE_CURVE('',#4850,#4921,#2236,.T.);
#6029=EDGE_CURVE('',#4921,#4920,#2820,.T.);
#6030=EDGE_CURVE('',#4922,#4923,#2237,.T.);
#6031=EDGE_CURVE('',#4923,#4924,#2238,.T.);
#6032=EDGE_CURVE('',#4924,#4925,#2239,.T.);
#6033=EDGE_CURVE('',#4925,#4926,#2821,.T.);
#6034=EDGE_CURVE('',#4926,#4922,#2240,.T.);
#6035=EDGE_CURVE('',#4851,#4927,#2241,.T.);
#6036=EDGE_CURVE('',#4927,#4928,#2242,.T.);
#6037=EDGE_CURVE('',#4929,#4928,#2822,.T.);
#6038=EDGE_CURVE('',#4929,#4930,#2243,.T.);
#6039=EDGE_CURVE('',#4930,#4852,#2244,.T.);
#6040=EDGE_CURVE('',#4931,#4932,#2245,.T.);
#6041=EDGE_CURVE('',#4932,#4933,#2246,.T.);
#6042=EDGE_CURVE('',#4933,#4934,#2247,.T.);
#6043=EDGE_CURVE('',#4934,#4935,#2248,.T.);
#6044=EDGE_CURVE('',#4935,#4931,#2823,.T.);
#6045=EDGE_CURVE('',#4936,#4937,#2824,.T.);
#6046=EDGE_CURVE('',#4937,#4938,#125,.T.);
#6047=EDGE_CURVE('',#4938,#4939,#2825,.T.);
#6048=EDGE_CURVE('',#4939,#4940,#126,.T.);
#6049=EDGE_CURVE('',#4940,#4941,#2826,.T.);
#6050=EDGE_CURVE('',#4941,#4942,#127,.T.);
#6051=EDGE_CURVE('',#4942,#4943,#2827,.T.);
#6052=EDGE_CURVE('',#4943,#4936,#128,.T.);
#6053=EDGE_CURVE('',#4944,#4945,#2828,.T.);
#6054=EDGE_CURVE('',#4946,#4944,#129,.T.);
#6055=EDGE_CURVE('',#4947,#4946,#2829,.T.);
#6056=EDGE_CURVE('',#4948,#4947,#130,.T.);
#6057=EDGE_CURVE('',#4949,#4948,#2830,.T.);
#6058=EDGE_CURVE('',#4950,#4949,#131,.T.);
#6059=EDGE_CURVE('',#4951,#4950,#2831,.T.);
#6060=EDGE_CURVE('',#4945,#4951,#132,.T.);
#6061=EDGE_CURVE('',#4928,#4952,#2249,.T.);
#6062=EDGE_CURVE('',#4952,#4943,#2832,.T.);
#6063=EDGE_CURVE('',#4942,#4953,#2833,.T.);
#6064=EDGE_CURVE('',#4953,#4929,#2250,.T.);
#6065=EDGE_CURVE('',#4940,#4954,#2834,.T.);
#6066=EDGE_CURVE('',#4954,#4955,#2251,.T.);
#6067=EDGE_CURVE('',#4955,#4956,#2835,.T.);
#6068=EDGE_CURVE('',#4956,#4941,#2836,.T.);
#6069=EDGE_CURVE('',#4957,#4958,#2837,.T.);
#6070=EDGE_CURVE('',#4958,#4959,#2252,.T.);
#6071=EDGE_CURVE('',#4959,#4937,#2838,.T.);
#6072=EDGE_CURVE('',#4936,#4957,#2839,.T.);
#6073=EDGE_CURVE('',#4938,#4960,#2840,.T.);
#6074=EDGE_CURVE('',#4960,#4961,#2841,.T.);
#6075=EDGE_CURVE('',#4961,#4939,#2842,.T.);
#6076=EDGE_CURVE('',#4955,#4926,#2712,.T.);
#6077=EDGE_CURVE('',#4925,#4962,#2253,.T.);
#6078=EDGE_CURVE('',#4962,#4956,#2254,.T.);
#6079=EDGE_CURVE('',#4963,#4964,#2713,.T.);
#6080=EDGE_CURVE('',#4964,#4920,#2255,.T.);
#6081=EDGE_CURVE('',#4921,#4965,#2256,.T.);
#6082=EDGE_CURVE('',#4965,#4966,#2714,.T.);
#6083=EDGE_CURVE('',#4966,#4961,#2257,.T.);
#6084=EDGE_CURVE('',#4960,#4963,#2258,.T.);
#6085=EDGE_CURVE('',#4935,#4958,#2715,.T.);
#6086=EDGE_CURVE('',#4957,#4967,#2259,.T.);
#6087=EDGE_CURVE('',#4967,#4931,#2260,.T.);
#6088=EDGE_CURVE('',#4960,#4959,#2261,.T.);
#6089=EDGE_CURVE('',#4963,#4958,#2262,.T.);
#6090=EDGE_CURVE('',#4964,#4935,#2263,.T.);
#6091=EDGE_CURVE('',#4920,#4934,#2264,.T.);
#6092=EDGE_CURVE('',#4933,#4846,#2716,.T.);
#6093=EDGE_CURVE('',#4954,#4961,#2265,.T.);
#6094=EDGE_CURVE('',#4955,#4966,#2266,.T.);
#6095=EDGE_CURVE('',#4926,#4965,#2267,.T.);
#6096=EDGE_CURVE('',#4922,#4921,#2268,.T.);
#6097=EDGE_CURVE('',#4850,#4923,#2717,.T.);
#6098=EDGE_CURVE('',#4957,#4952,#2269,.T.);
#6099=EDGE_CURVE('',#4967,#4928,#2270,.T.);
#6100=EDGE_CURVE('',#4931,#4927,#2271,.T.);
#6101=EDGE_CURVE('',#4851,#4932,#2718,.T.);
#6102=EDGE_CURVE('',#4953,#4956,#2272,.T.);
#6103=EDGE_CURVE('',#4929,#4962,#2273,.T.);
#6104=EDGE_CURVE('',#4930,#4925,#2274,.T.);
#6105=EDGE_CURVE('',#4924,#4852,#2719,.T.);
#6106=EDGE_CURVE('',#4854,#4924,#2275,.T.);
#6107=EDGE_CURVE('',#4855,#4923,#2276,.T.);
#6108=EDGE_CURVE('',#4856,#4933,#2277,.T.);
#6109=EDGE_CURVE('',#4857,#4932,#2278,.T.);
#6110=EDGE_CURVE('',#4840,#4770,#2279,.T.);
#6111=EDGE_CURVE('',#4968,#4837,#2280,.T.);
#6112=EDGE_CURVE('',#4969,#4968,#2843,.T.);
#6113=EDGE_CURVE('',#4838,#4969,#2281,.T.);
#6114=EDGE_CURVE('',#4970,#4971,#2282,.T.);
#6115=EDGE_CURVE('',#4972,#4970,#2283,.T.);
#6116=EDGE_CURVE('',#4973,#4972,#2844,.T.);
#6117=EDGE_CURVE('',#4974,#4973,#2284,.T.);
#6118=EDGE_CURVE('',#4971,#4974,#2285,.T.);
#6119=EDGE_CURVE('',#4975,#4843,#2286,.T.);
#6120=EDGE_CURVE('',#4976,#4975,#2287,.T.);
#6121=EDGE_CURVE('',#4976,#4977,#2845,.T.);
#6122=EDGE_CURVE('',#4978,#4977,#2288,.T.);
#6123=EDGE_CURVE('',#4768,#4978,#2289,.T.);
#6124=EDGE_CURVE('',#4979,#4980,#2290,.T.);
#6125=EDGE_CURVE('',#4981,#4979,#2846,.T.);
#6126=EDGE_CURVE('',#4982,#4981,#2291,.T.);
#6127=EDGE_CURVE('',#4983,#4982,#2292,.T.);
#6128=EDGE_CURVE('',#4980,#4983,#2293,.T.);
#6129=EDGE_CURVE('',#4984,#4976,#2294,.T.);
#6130=EDGE_CURVE('',#4947,#4984,#2847,.T.);
#6131=EDGE_CURVE('',#4985,#4946,#2848,.T.);
#6132=EDGE_CURVE('',#4977,#4985,#2295,.T.);
#6133=EDGE_CURVE('',#4949,#4986,#2849,.T.);
#6134=EDGE_CURVE('',#4987,#4948,#2850,.T.);
#6135=EDGE_CURVE('',#4988,#4987,#2851,.T.);
#6136=EDGE_CURVE('',#4986,#4988,#2296,.T.);
#6137=EDGE_CURVE('',#4989,#4990,#2852,.T.);
#6138=EDGE_CURVE('',#4944,#4989,#2853,.T.);
#6139=EDGE_CURVE('',#4991,#4945,#2854,.T.);
#6140=EDGE_CURVE('',#4990,#4991,#2297,.T.);
#6141=EDGE_CURVE('',#4992,#4950,#2855,.T.);
#6142=EDGE_CURVE('',#4993,#4992,#2856,.T.);
#6143=EDGE_CURVE('',#4951,#4993,#2857,.T.);
#6144=EDGE_CURVE('',#4994,#4987,#2298,.T.);
#6145=EDGE_CURVE('',#4973,#4994,#2299,.T.);
#6146=EDGE_CURVE('',#4988,#4972,#2720,.T.);
#6147=EDGE_CURVE('',#4995,#4996,#2721,.T.);
#6148=EDGE_CURVE('',#4993,#4995,#2300,.T.);
#6149=EDGE_CURVE('',#4997,#4992,#2301,.T.);
#6150=EDGE_CURVE('',#4998,#4997,#2722,.T.);
#6151=EDGE_CURVE('',#4969,#4998,#2302,.T.);
#6152=EDGE_CURVE('',#4996,#4968,#2303,.T.);
#6153=EDGE_CURVE('',#4999,#4979,#2304,.T.);
#6154=EDGE_CURVE('',#4989,#4999,#2305,.T.);
#6155=EDGE_CURVE('',#4981,#4990,#2723,.T.);
#6156=EDGE_CURVE('',#4993,#4991,#2306,.T.);
#6157=EDGE_CURVE('',#4995,#4990,#2307,.T.);
#6158=EDGE_CURVE('',#4996,#4981,#2308,.T.);
#6159=EDGE_CURVE('',#4968,#4982,#2309,.T.);
#6160=EDGE_CURVE('',#4983,#4837,#2724,.T.);
#6161=EDGE_CURVE('',#4986,#4992,#2310,.T.);
#6162=EDGE_CURVE('',#4988,#4997,#2311,.T.);
#6163=EDGE_CURVE('',#4972,#4998,#2312,.T.);
#6164=EDGE_CURVE('',#4970,#4969,#2313,.T.);
#6165=EDGE_CURVE('',#4838,#4971,#2725,.T.);
#6166=EDGE_CURVE('',#4989,#4985,#2314,.T.);
#6167=EDGE_CURVE('',#4999,#4977,#2315,.T.);
#6168=EDGE_CURVE('',#4979,#4978,#2316,.T.);
#6169=EDGE_CURVE('',#4768,#4980,#2726,.T.);
#6170=EDGE_CURVE('',#4984,#4987,#2317,.T.);
#6171=EDGE_CURVE('',#4976,#4994,#2318,.T.);
#6172=EDGE_CURVE('',#4975,#4973,#2319,.T.);
#6173=EDGE_CURVE('',#4974,#4843,#2727,.T.);
#6174=EDGE_CURVE('',#4842,#4974,#2320,.T.);
#6175=EDGE_CURVE('',#4841,#4971,#2321,.T.);
#6176=EDGE_CURVE('',#4840,#4983,#2322,.T.);
#6177=EDGE_CURVE('',#4770,#4980,#2323,.T.);
#6178=EDGE_CURVE('',#5000,#5001,#2858,.T.);
#6179=EDGE_CURVE('',#5001,#5002,#2859,.T.);
#6180=EDGE_CURVE('',#5002,#5003,#2860,.T.);
#6181=EDGE_CURVE('',#5003,#5000,#2861,.T.);
#6182=EDGE_CURVE('',#5004,#5005,#2862,.T.);
#6183=EDGE_CURVE('',#5005,#5006,#2863,.T.);
#6184=EDGE_CURVE('',#5006,#5007,#2864,.T.);
#6185=EDGE_CURVE('',#5007,#5008,#2865,.T.);
#6186=EDGE_CURVE('',#5008,#5009,#2866,.T.);
#6187=EDGE_CURVE('',#5009,#5004,#2867,.T.);
#6188=EDGE_CURVE('',#5010,#5011,#2868,.T.);
#6189=EDGE_CURVE('',#5011,#5012,#2869,.T.);
#6190=EDGE_CURVE('',#5012,#5013,#2870,.T.);
#6191=EDGE_CURVE('',#5013,#5010,#2324,.T.);
#6192=EDGE_CURVE('',#5014,#5015,#2871,.T.);
#6193=EDGE_CURVE('',#5015,#5016,#2325,.T.);
#6194=EDGE_CURVE('',#5016,#5017,#2872,.T.);
#6195=EDGE_CURVE('',#5017,#5014,#2873,.T.);
#6196=EDGE_CURVE('',#5018,#5019,#2874,.T.);
#6197=EDGE_CURVE('',#5019,#5020,#2875,.T.);
#6198=EDGE_CURVE('',#5020,#5021,#2876,.T.);
#6199=EDGE_CURVE('',#5021,#5018,#2877,.T.);
#6200=EDGE_CURVE('',#5022,#5023,#2878,.T.);
#6201=EDGE_CURVE('',#5023,#5024,#2326,.T.);
#6202=EDGE_CURVE('',#5024,#5022,#2879,.T.);
#6203=EDGE_CURVE('',#5025,#5026,#2880,.T.);
#6204=EDGE_CURVE('',#5026,#5027,#2327,.T.);
#6205=EDGE_CURVE('',#5027,#5025,#2881,.T.);
#6206=EDGE_CURVE('',#5028,#5029,#2882,.T.);
#6207=EDGE_CURVE('',#5029,#5030,#2883,.T.);
#6208=EDGE_CURVE('',#5030,#5031,#2884,.T.);
#6209=EDGE_CURVE('',#5031,#5028,#2885,.T.);
#6210=EDGE_CURVE('',#5032,#5033,#2886,.T.);
#6211=EDGE_CURVE('',#5033,#5034,#2328,.T.);
#6212=EDGE_CURVE('',#5034,#5032,#2887,.T.);
#6213=EDGE_CURVE('',#5035,#5036,#2888,.T.);
#6214=EDGE_CURVE('',#5036,#5037,#2329,.T.);
#6215=EDGE_CURVE('',#5037,#5035,#2889,.T.);
#6216=EDGE_CURVE('',#5038,#5039,#2890,.T.);
#6217=EDGE_CURVE('',#5039,#5040,#2891,.T.);
#6218=EDGE_CURVE('',#5040,#5041,#2892,.T.);
#6219=EDGE_CURVE('',#5041,#5038,#2893,.T.);
#6220=EDGE_CURVE('',#5042,#5043,#2894,.T.);
#6221=EDGE_CURVE('',#5043,#5044,#2895,.T.);
#6222=EDGE_CURVE('',#5044,#5045,#2330,.T.);
#6223=EDGE_CURVE('',#5045,#5042,#2896,.T.);
#6224=EDGE_CURVE('',#5046,#5047,#2897,.T.);
#6225=EDGE_CURVE('',#5047,#5048,#2331,.T.);
#6226=EDGE_CURVE('',#5048,#5049,#2898,.T.);
#6227=EDGE_CURVE('',#5049,#5046,#2899,.T.);
#6228=EDGE_CURVE('',#5050,#5051,#2900,.T.);
#6229=EDGE_CURVE('',#5051,#5052,#2901,.T.);
#6230=EDGE_CURVE('',#5052,#5053,#2902,.T.);
#6231=EDGE_CURVE('',#5053,#5050,#2903,.T.);
#6232=EDGE_CURVE('',#5054,#5055,#2904,.T.);
#6233=EDGE_CURVE('',#5055,#4798,#2332,.T.);
#6234=EDGE_CURVE('',#4798,#5054,#2905,.T.);
#6235=EDGE_CURVE('',#5056,#4794,#2906,.T.);
#6236=EDGE_CURVE('',#4794,#5057,#2333,.T.);
#6237=EDGE_CURVE('',#5057,#5056,#2907,.T.);
#6238=EDGE_CURVE('',#5058,#5059,#2908,.T.);
#6239=EDGE_CURVE('',#5059,#5060,#2909,.T.);
#6240=EDGE_CURVE('',#5060,#5061,#2910,.T.);
#6241=EDGE_CURVE('',#5061,#5058,#2911,.T.);
#6242=EDGE_CURVE('',#5062,#4787,#2912,.T.);
#6243=EDGE_CURVE('',#4787,#5063,#2334,.T.);
#6244=EDGE_CURVE('',#5063,#5062,#2913,.T.);
#6245=EDGE_CURVE('',#5064,#5065,#2914,.T.);
#6246=EDGE_CURVE('',#5065,#4792,#2335,.T.);
#6247=EDGE_CURVE('',#4792,#5064,#2915,.T.);
#6248=EDGE_CURVE('',#5066,#5067,#2916,.T.);
#6249=EDGE_CURVE('',#5067,#5068,#2917,.T.);
#6250=EDGE_CURVE('',#5068,#5069,#2918,.T.);
#6251=EDGE_CURVE('',#5069,#5066,#2919,.T.);
#6252=EDGE_CURVE('',#5070,#5071,#2920,.T.);
#6253=EDGE_CURVE('',#5071,#5072,#2921,.T.);
#6254=EDGE_CURVE('',#5072,#5073,#2922,.T.);
#6255=EDGE_CURVE('',#5073,#5070,#2923,.T.);
#6256=EDGE_CURVE('',#5074,#5075,#2924,.T.);
#6257=EDGE_CURVE('',#5075,#5076,#2925,.T.);
#6258=EDGE_CURVE('',#5076,#5077,#2926,.T.);
#6259=EDGE_CURVE('',#5077,#5074,#2927,.T.);
#6260=EDGE_CURVE('',#5078,#5079,#2928,.T.);
#6261=EDGE_CURVE('',#5079,#5080,#2929,.T.);
#6262=EDGE_CURVE('',#5080,#5081,#2930,.T.);
#6263=EDGE_CURVE('',#5081,#5078,#2931,.T.);
#6264=EDGE_CURVE('',#5054,#4906,#2336,.T.);
#6265=EDGE_CURVE('',#5055,#5053,#2728,.T.);
#6266=EDGE_CURVE('',#5050,#5054,#2337,.T.);
#6267=EDGE_CURVE('',#4872,#5055,#2338,.T.);
#6268=EDGE_CURVE('',#5073,#5040,#2339,.T.);
#6269=EDGE_CURVE('',#4893,#5073,#2340,.T.);
#6270=EDGE_CURVE('',#5040,#4893,#2341,.T.);
#6271=EDGE_CURVE('',#4894,#5071,#2342,.T.);
#6272=EDGE_CURVE('',#5046,#4894,#2343,.T.);
#6273=EDGE_CURVE('',#5071,#5046,#2344,.T.);
#6274=EDGE_CURVE('',#5050,#4905,#2345,.T.);
#6275=EDGE_CURVE('',#4873,#5053,#2346,.T.);
#6276=EDGE_CURVE('',#4907,#4887,#2347,.T.);
#6277=EDGE_CURVE('',#5047,#4907,#2729,.T.);
#6278=EDGE_CURVE('',#5072,#5049,#2348,.T.);
#6279=EDGE_CURVE('',#4888,#5072,#2349,.T.);
#6280=EDGE_CURVE('',#5041,#4892,#2350,.T.);
#6281=EDGE_CURVE('',#5070,#5039,#2351,.T.);
#6282=EDGE_CURVE('',#4895,#5070,#2352,.T.);
#6283=EDGE_CURVE('',#5051,#4904,#2353,.T.);
#6284=EDGE_CURVE('',#5052,#5057,#2730,.T.);
#6285=EDGE_CURVE('',#5056,#5051,#2354,.T.);
#6286=EDGE_CURVE('',#4874,#5052,#2355,.T.);
#6287=EDGE_CURVE('',#5047,#4886,#2356,.T.);
#6288=EDGE_CURVE('',#4888,#5049,#2357,.T.);
#6289=EDGE_CURVE('',#5041,#5068,#2358,.T.);
#6290=EDGE_CURVE('',#5068,#4892,#2359,.T.);
#6291=EDGE_CURVE('',#4895,#5039,#2360,.T.);
#6292=EDGE_CURVE('',#5056,#4903,#2361,.T.);
#6293=EDGE_CURVE('',#4875,#5057,#2362,.T.);
#6294=EDGE_CURVE('',#5048,#4885,#2363,.T.);
#6295=EDGE_CURVE('',#4889,#5048,#2731,.T.);
#6296=EDGE_CURVE('',#5069,#4891,#2364,.T.);
#6297=EDGE_CURVE('',#5038,#5067,#2365,.T.);
#6298=EDGE_CURVE('',#4896,#5038,#2366,.T.);
#6299=EDGE_CURVE('',#4889,#4884,#2367,.T.);
#6300=EDGE_CURVE('',#5069,#5043,#2368,.T.);
#6301=EDGE_CURVE('',#5043,#4891,#2369,.T.);
#6302=EDGE_CURVE('',#4896,#5067,#2370,.T.);
#6303=EDGE_CURVE('',#4890,#4883,#2371,.T.);
#6304=EDGE_CURVE('',#5044,#4890,#2732,.T.);
#6305=EDGE_CURVE('',#5066,#5042,#2372,.T.);
#6306=EDGE_CURVE('',#4897,#5066,#2373,.T.);
#6307=EDGE_CURVE('',#5064,#4902,#2374,.T.);
#6308=EDGE_CURVE('',#5044,#4882,#2375,.T.);
#6309=EDGE_CURVE('',#4897,#5042,#2376,.T.);
#6310=EDGE_CURVE('',#5058,#4901,#2377,.T.);
#6311=EDGE_CURVE('',#5064,#5058,#2378,.T.);
#6312=EDGE_CURVE('',#5045,#4881,#2379,.T.);
#6313=EDGE_CURVE('',#4898,#5045,#2733,.T.);
#6314=EDGE_CURVE('',#5059,#4900,#2380,.T.);
#6315=EDGE_CURVE('',#5065,#5061,#2734,.T.);
#6316=EDGE_CURVE('',#4876,#5065,#2381,.T.);
#6317=EDGE_CURVE('',#4898,#4880,#2382,.T.);
#6318=EDGE_CURVE('',#5062,#4899,#2383,.T.);
#6319=EDGE_CURVE('',#5059,#5062,#2384,.T.);
#6320=EDGE_CURVE('',#4877,#5061,#2385,.T.);
#6321=EDGE_CURVE('',#5060,#5063,#2735,.T.);
#6322=EDGE_CURVE('',#4878,#5060,#2386,.T.);
#6323=EDGE_CURVE('',#4879,#5063,#2387,.T.);
#6324=EDGE_CURVE('',#5079,#5008,#2388,.T.);
#6325=EDGE_CURVE('',#5001,#5079,#2389,.T.);
#6326=EDGE_CURVE('',#5008,#5001,#2390,.T.);
#6327=EDGE_CURVE('',#5078,#4911,#2391,.T.);
#6328=EDGE_CURVE('',#4912,#5081,#2392,.T.);
#6329=EDGE_CURVE('',#5002,#5078,#2393,.T.);
#6330=EDGE_CURVE('',#5009,#5000,#2394,.T.);
#6331=EDGE_CURVE('',#5080,#5007,#2395,.T.);
#6332=EDGE_CURVE('',#5081,#5017,#2396,.T.);
#6333=EDGE_CURVE('',#5014,#5080,#2397,.T.);
#6334=EDGE_CURVE('',#4912,#5017,#2398,.T.);
#6335=EDGE_CURVE('',#5002,#4911,#2399,.T.);
#6336=EDGE_CURVE('',#5009,#5075,#2400,.T.);
#6337=EDGE_CURVE('',#5075,#5000,#2401,.T.);
#6338=EDGE_CURVE('',#5014,#5007,#2402,.T.);
#6339=EDGE_CURVE('',#4785,#5016,#2736,.T.);
#6340=EDGE_CURVE('',#5003,#4910,#2403,.T.);
#6341=EDGE_CURVE('',#5076,#5003,#2404,.T.);
#6342=EDGE_CURVE('',#5004,#5074,#2405,.T.);
#6343=EDGE_CURVE('',#5015,#5006,#2737,.T.);
#6344=EDGE_CURVE('',#4863,#5015,#2406,.T.);
#6345=EDGE_CURVE('',#5016,#4862,#2407,.T.);
#6346=EDGE_CURVE('',#5076,#4910,#2408,.T.);
#6347=EDGE_CURVE('',#5004,#5011,#2409,.T.);
#6348=EDGE_CURVE('',#5011,#5074,#2410,.T.);
#6349=EDGE_CURVE('',#4864,#5006,#2411,.T.);
#6350=EDGE_CURVE('',#5077,#4909,#2412,.T.);
#6351=EDGE_CURVE('',#5012,#5077,#2413,.T.);
#6352=EDGE_CURVE('',#5005,#5010,#2738,.T.);
#6353=EDGE_CURVE('',#4865,#5005,#2414,.T.);
#6354=EDGE_CURVE('',#4783,#5023,#2415,.T.);
#6355=EDGE_CURVE('',#5023,#4784,#2416,.T.);
#6356=EDGE_CURVE('',#5012,#4909,#2417,.T.);
#6357=EDGE_CURVE('',#4866,#5010,#2418,.T.);
#6358=EDGE_CURVE('',#5024,#4861,#2419,.T.);
#6359=EDGE_CURVE('',#5022,#5018,#2420,.T.);
#6360=EDGE_CURVE('',#5019,#5024,#2739,.T.);
#6361=EDGE_CURVE('',#4913,#5022,#2421,.T.);
#6362=EDGE_CURVE('',#5013,#4780,#2740,.T.);
#6363=EDGE_CURVE('',#4867,#5013,#2422,.T.);
#6364=EDGE_CURVE('',#5019,#4860,#2423,.T.);
#6365=EDGE_CURVE('',#4914,#5018,#2424,.T.);
#6366=EDGE_CURVE('',#5020,#4859,#2425,.T.);
#6367=EDGE_CURVE('',#5021,#5025,#2426,.T.);
#6368=EDGE_CURVE('',#5026,#5020,#2741,.T.);
#6369=EDGE_CURVE('',#4915,#5021,#2427,.T.);
#6370=EDGE_CURVE('',#4781,#5034,#2428,.T.);
#6371=EDGE_CURVE('',#5032,#4908,#2429,.T.);
#6372=EDGE_CURVE('',#5026,#4858,#2430,.T.);
#6373=EDGE_CURVE('',#4916,#5025,#2431,.T.);
#6374=EDGE_CURVE('',#5031,#4919,#2432,.T.);
#6375=EDGE_CURVE('',#5032,#5031,#2433,.T.);
#6376=EDGE_CURVE('',#4782,#5034,#2434,.T.);
#6377=EDGE_CURVE('',#5027,#4777,#2435,.T.);
#6378=EDGE_CURVE('',#4776,#5027,#2436,.T.);
#6379=EDGE_CURVE('',#5028,#4918,#2437,.T.);
#6380=EDGE_CURVE('',#5033,#5030,#2742,.T.);
#6381=EDGE_CURVE('',#4868,#5033,#2438,.T.);
#6382=EDGE_CURVE('',#5035,#4917,#2439,.T.);
#6383=EDGE_CURVE('',#5028,#5035,#2440,.T.);
#6384=EDGE_CURVE('',#4869,#5030,#2441,.T.);
#6385=EDGE_CURVE('',#5036,#4774,#2442,.T.);
#6386=EDGE_CURVE('',#5029,#5037,#2743,.T.);
#6387=EDGE_CURVE('',#4870,#5029,#2443,.T.);
#6388=EDGE_CURVE('',#5036,#4775,#2444,.T.);
#6389=EDGE_CURVE('',#4871,#5037,#2445,.T.);
#6390=EDGE_CURVE('',#5082,#5082,#2446,.T.);
#6391=EDGE_CURVE('',#5082,#5083,#2932,.T.);
#6392=EDGE_CURVE('',#5084,#5083,#2447,.T.);
#6393=EDGE_CURVE('',#5083,#5084,#2448,.T.);
#6394=EDGE_CURVE('',#5085,#5086,#2449,.T.);
#6395=EDGE_CURVE('',#5086,#5085,#2450,.T.);
#6396=EDGE_CURVE('',#5086,#5087,#2933,.T.);
#6397=EDGE_CURVE('',#5087,#5087,#2451,.T.);
#6398=EDGE_CURVE('',#5088,#5089,#2452,.T.);
#6399=EDGE_CURVE('',#5089,#5088,#2453,.T.);
#6400=EDGE_CURVE('',#5089,#5090,#2934,.T.);
#6401=EDGE_CURVE('',#5090,#5090,#2454,.T.);
#6402=EDGE_CURVE('',#5091,#5092,#2455,.T.);
#6403=EDGE_CURVE('',#5092,#5093,#2935,.T.);
#6404=EDGE_CURVE('',#5093,#5094,#2456,.T.);
#6405=EDGE_CURVE('',#5091,#5094,#2936,.T.);
#6406=EDGE_CURVE('',#5095,#5095,#2457,.T.);
#6407=EDGE_CURVE('',#5095,#5096,#2937,.T.);
#6408=EDGE_CURVE('',#5097,#5096,#2458,.T.);
#6409=EDGE_CURVE('',#5098,#5097,#2459,.T.);
#6410=EDGE_CURVE('',#5099,#5098,#2460,.T.);
#6411=EDGE_CURVE('',#5100,#5099,#2461,.T.);
#6412=EDGE_CURVE('',#5101,#5100,#2462,.T.);
#6413=EDGE_CURVE('',#5102,#5101,#2463,.T.);
#6414=EDGE_CURVE('',#5103,#5102,#2464,.T.);
#6415=EDGE_CURVE('',#5104,#5103,#2465,.T.);
#6416=EDGE_CURVE('',#5105,#5104,#2466,.T.);
#6417=EDGE_CURVE('',#5106,#5105,#2467,.T.);
#6418=EDGE_CURVE('',#5107,#5106,#2468,.T.);
#6419=EDGE_CURVE('',#5108,#5107,#2469,.T.);
#6420=EDGE_CURVE('',#5109,#5108,#2470,.T.);
#6421=EDGE_CURVE('',#5110,#5109,#2471,.T.);
#6422=EDGE_CURVE('',#5111,#5110,#2472,.T.);
#6423=EDGE_CURVE('',#5112,#5111,#2473,.T.);
#6424=EDGE_CURVE('',#5113,#5112,#2474,.T.);
#6425=EDGE_CURVE('',#5113,#5114,#2475,.T.);
#6426=EDGE_CURVE('',#5115,#5114,#2476,.T.);
#6427=EDGE_CURVE('',#5116,#5115,#2477,.T.);
#6428=EDGE_CURVE('',#5096,#5116,#2478,.T.);
#6429=EDGE_CURVE('',#5117,#5117,#2479,.T.);
#6430=EDGE_CURVE('',#5117,#5118,#2938,.T.);
#6431=EDGE_CURVE('',#5119,#5118,#2480,.T.);
#6432=EDGE_CURVE('',#5120,#5119,#2939,.T.);
#6433=EDGE_CURVE('',#5120,#5121,#2481,.T.);
#6434=EDGE_CURVE('',#5121,#5122,#2940,.T.);
#6435=EDGE_CURVE('',#5122,#5122,#2482,.T.);
#6436=EDGE_CURVE('',#5121,#5123,#2483,.T.);
#6437=EDGE_CURVE('',#5123,#5124,#2941,.T.);
#6438=EDGE_CURVE('',#5118,#5124,#2484,.T.);
#6439=EDGE_CURVE('',#5125,#5126,#2485,.T.);
#6440=EDGE_CURVE('',#5126,#5127,#2942,.T.);
#6441=EDGE_CURVE('',#5128,#5127,#2486,.T.);
#6442=EDGE_CURVE('',#5125,#5128,#2943,.T.);
#6443=EDGE_CURVE('',#5129,#5130,#2944,.T.);
#6444=EDGE_CURVE('',#5129,#5131,#2487,.T.);
#6445=EDGE_CURVE('',#5131,#5132,#2945,.T.);
#6446=EDGE_CURVE('',#5130,#5132,#2488,.T.);
#6447=EDGE_CURVE('',#5133,#5134,#2946,.T.);
#6448=EDGE_CURVE('',#5133,#5135,#2489,.T.);
#6449=EDGE_CURVE('',#5135,#5136,#2947,.T.);
#6450=EDGE_CURVE('',#5134,#5136,#2490,.T.);
#6451=EDGE_CURVE('',#5137,#5138,#2948,.T.);
#6452=EDGE_CURVE('',#5137,#5139,#2491,.T.);
#6453=EDGE_CURVE('',#5139,#5140,#2949,.T.);
#6454=EDGE_CURVE('',#5138,#5140,#2492,.T.);
#6455=EDGE_CURVE('',#5141,#5142,#2950,.T.);
#6456=EDGE_CURVE('',#5141,#5143,#2493,.T.);
#6457=EDGE_CURVE('',#5143,#5144,#2951,.T.);
#6458=EDGE_CURVE('',#5142,#5144,#2494,.T.);
#6459=EDGE_CURVE('',#5145,#5146,#2495,.T.);
#6460=EDGE_CURVE('',#5146,#5147,#2952,.T.);
#6461=EDGE_CURVE('',#5148,#5147,#2496,.T.);
#6462=EDGE_CURVE('',#5145,#5148,#2953,.T.);
#6463=EDGE_CURVE('',#5149,#5150,#2954,.T.);
#6464=EDGE_CURVE('',#5149,#5151,#2497,.T.);
#6465=EDGE_CURVE('',#5151,#5152,#2955,.T.);
#6466=EDGE_CURVE('',#5150,#5152,#2498,.T.);
#6467=EDGE_CURVE('',#5153,#5154,#2956,.T.);
#6468=EDGE_CURVE('',#5153,#5155,#2499,.T.);
#6469=EDGE_CURVE('',#5155,#5156,#2957,.T.);
#6470=EDGE_CURVE('',#5154,#5156,#2500,.T.);
#6471=EDGE_CURVE('',#5157,#5158,#2958,.T.);
#6472=EDGE_CURVE('',#5157,#5159,#2501,.T.);
#6473=EDGE_CURVE('',#5159,#5160,#2959,.T.);
#6474=EDGE_CURVE('',#5158,#5160,#2502,.T.);
#6475=EDGE_CURVE('',#5088,#5084,#2960,.T.);
#6476=EDGE_CURVE('',#5085,#5161,#2961,.T.);
#6477=EDGE_CURVE('',#5161,#5161,#2503,.T.);
#6478=EDGE_CURVE('',#5111,#5162,#2962,.T.);
#6479=EDGE_CURVE('',#5162,#5163,#2963,.T.);
#6480=EDGE_CURVE('',#5163,#5112,#2964,.T.);
#6481=EDGE_CURVE('',#5109,#5164,#2965,.T.);
#6482=EDGE_CURVE('',#5164,#5165,#2966,.T.);
#6483=EDGE_CURVE('',#5165,#5110,#2967,.T.);
#6484=EDGE_CURVE('',#5107,#5166,#2968,.T.);
#6485=EDGE_CURVE('',#5166,#5167,#2969,.T.);
#6486=EDGE_CURVE('',#5167,#5108,#2970,.T.);
#6487=EDGE_CURVE('',#5105,#5168,#2971,.T.);
#6488=EDGE_CURVE('',#5168,#5169,#2972,.T.);
#6489=EDGE_CURVE('',#5169,#5106,#2973,.T.);
#6490=EDGE_CURVE('',#5103,#5170,#2974,.T.);
#6491=EDGE_CURVE('',#5170,#5171,#2975,.T.);
#6492=EDGE_CURVE('',#5171,#5104,#2976,.T.);
#6493=EDGE_CURVE('',#5101,#5172,#2977,.T.);
#6494=EDGE_CURVE('',#5172,#5173,#2978,.T.);
#6495=EDGE_CURVE('',#5173,#5102,#2979,.T.);
#6496=EDGE_CURVE('',#5099,#5174,#2980,.T.);
#6497=EDGE_CURVE('',#5174,#5175,#2981,.T.);
#6498=EDGE_CURVE('',#5175,#5100,#2982,.T.);
#6499=EDGE_CURVE('',#5097,#5176,#2983,.T.);
#6500=EDGE_CURVE('',#5176,#5177,#2984,.T.);
#6501=EDGE_CURVE('',#5177,#5098,#2985,.T.);
#6502=EDGE_CURVE('',#5115,#5178,#2986,.T.);
#6503=EDGE_CURVE('',#5178,#5179,#2987,.T.);
#6504=EDGE_CURVE('',#5179,#5116,#2988,.T.);
#6505=EDGE_CURVE('',#5113,#5180,#2989,.T.);
#6506=EDGE_CURVE('',#5180,#5181,#2990,.T.);
#6507=EDGE_CURVE('',#5181,#5114,#2991,.T.);
#6508=EDGE_CURVE('',#5182,#5152,#2992,.T.);
#6509=EDGE_CURVE('',#5183,#5182,#2504,.T.);
#6510=EDGE_CURVE('',#5184,#5183,#2993,.T.);
#6511=EDGE_CURVE('',#5185,#5184,#2994,.T.);
#6512=EDGE_CURVE('',#5148,#5185,#2995,.T.);
#6513=EDGE_CURVE('',#5186,#5147,#2996,.T.);
#6514=EDGE_CURVE('',#5187,#5186,#2505,.T.);
#6515=EDGE_CURVE('',#5188,#5187,#2997,.T.);
#6516=EDGE_CURVE('',#5189,#5188,#2998,.T.);
#6517=EDGE_CURVE('',#5158,#5189,#2999,.T.);
#6518=EDGE_CURVE('',#5190,#5160,#3000,.T.);
#6519=EDGE_CURVE('',#5191,#5190,#2506,.T.);
#6520=EDGE_CURVE('',#5192,#5191,#3001,.T.);
#6521=EDGE_CURVE('',#5193,#5192,#3002,.T.);
#6522=EDGE_CURVE('',#5154,#5193,#3003,.T.);
#6523=EDGE_CURVE('',#5194,#5156,#3004,.T.);
#6524=EDGE_CURVE('',#5195,#5194,#2507,.T.);
#6525=EDGE_CURVE('',#5196,#5195,#3005,.T.);
#6526=EDGE_CURVE('',#5197,#5196,#3006,.T.);
#6527=EDGE_CURVE('',#5128,#5197,#3007,.T.);
#6528=EDGE_CURVE('',#5198,#5127,#3008,.T.);
#6529=EDGE_CURVE('',#5199,#5198,#2508,.T.);
#6530=EDGE_CURVE('',#5200,#5199,#3009,.T.);
#6531=EDGE_CURVE('',#5201,#5200,#3010,.T.);
#6532=EDGE_CURVE('',#5142,#5201,#3011,.T.);
#6533=EDGE_CURVE('',#5202,#5144,#3012,.T.);
#6534=EDGE_CURVE('',#5203,#5202,#2509,.T.);
#6535=EDGE_CURVE('',#5204,#5203,#3013,.T.);
#6536=EDGE_CURVE('',#5205,#5204,#3014,.T.);
#6537=EDGE_CURVE('',#5138,#5205,#3015,.T.);
#6538=EDGE_CURVE('',#5206,#5140,#3016,.T.);
#6539=EDGE_CURVE('',#5207,#5206,#2510,.T.);
#6540=EDGE_CURVE('',#5208,#5207,#3017,.T.);
#6541=EDGE_CURVE('',#5209,#5208,#3018,.T.);
#6542=EDGE_CURVE('',#5134,#5209,#3019,.T.);
#6543=EDGE_CURVE('',#5210,#5136,#3020,.T.);
#6544=EDGE_CURVE('',#5211,#5210,#2511,.T.);
#6545=EDGE_CURVE('',#5212,#5211,#3021,.T.);
#6546=EDGE_CURVE('',#5213,#5212,#3022,.T.);
#6547=EDGE_CURVE('',#5130,#5213,#3023,.T.);
#6548=EDGE_CURVE('',#5214,#5132,#3024,.T.);
#6549=EDGE_CURVE('',#5215,#5214,#2512,.T.);
#6550=EDGE_CURVE('',#5216,#5215,#3025,.T.);
#6551=EDGE_CURVE('',#5217,#5216,#3026,.T.);
#6552=EDGE_CURVE('',#5119,#5217,#3027,.T.);
#6553=EDGE_CURVE('',#5218,#5124,#3028,.T.);
#6554=EDGE_CURVE('',#5219,#5218,#2513,.T.);
#6555=EDGE_CURVE('',#5220,#5219,#3029,.T.);
#6556=EDGE_CURVE('',#5221,#5220,#3030,.T.);
#6557=EDGE_CURVE('',#5150,#5221,#3031,.T.);
#6558=EDGE_CURVE('',#5092,#5222,#3032,.T.);
#6559=EDGE_CURVE('',#5223,#5091,#3033,.T.);
#6560=EDGE_CURVE('',#5222,#5223,#3034,.T.);
#6561=EDGE_CURVE('',#5224,#5093,#3035,.T.);
#6562=EDGE_CURVE('',#5225,#5224,#3036,.T.);
#6563=EDGE_CURVE('',#5094,#5225,#3037,.T.);
#6564=EDGE_CURVE('',#5226,#5188,#3038,.T.);
#6565=EDGE_CURVE('',#5226,#5227,#3039,.T.);
#6566=EDGE_CURVE('',#5227,#5189,#3040,.T.);
#6567=EDGE_CURVE('',#5163,#5226,#2514,.T.);
#6568=EDGE_CURVE('',#5228,#5187,#3041,.T.);
#6569=EDGE_CURVE('',#5112,#5228,#3042,.T.);
#6570=EDGE_CURVE('',#5229,#5186,#3043,.T.);
#6571=EDGE_CURVE('',#5228,#5229,#2515,.T.);
#6572=EDGE_CURVE('',#5229,#5146,#3044,.T.);
#6573=EDGE_CURVE('',#5227,#5162,#2516,.T.);
#6574=EDGE_CURVE('',#5157,#5111,#3045,.T.);
#6575=EDGE_CURVE('',#5230,#5192,#3046,.T.);
#6576=EDGE_CURVE('',#5230,#5231,#3047,.T.);
#6577=EDGE_CURVE('',#5231,#5193,#3048,.T.);
#6578=EDGE_CURVE('',#5165,#5230,#2517,.T.);
#6579=EDGE_CURVE('',#5232,#5191,#3049,.T.);
#6580=EDGE_CURVE('',#5110,#5232,#3050,.T.);
#6581=EDGE_CURVE('',#5233,#5190,#3051,.T.);
#6582=EDGE_CURVE('',#5232,#5233,#2518,.T.);
#6583=EDGE_CURVE('',#5233,#5159,#3052,.T.);
#6584=EDGE_CURVE('',#5231,#5164,#2519,.T.);
#6585=EDGE_CURVE('',#5153,#5109,#3053,.T.);
#6586=EDGE_CURVE('',#5234,#5196,#3054,.T.);
#6587=EDGE_CURVE('',#5234,#5235,#3055,.T.);
#6588=EDGE_CURVE('',#5235,#5197,#3056,.T.);
#6589=EDGE_CURVE('',#5167,#5234,#2520,.T.);
#6590=EDGE_CURVE('',#5236,#5195,#3057,.T.);
#6591=EDGE_CURVE('',#5108,#5236,#3058,.T.);
#6592=EDGE_CURVE('',#5237,#5194,#3059,.T.);
#6593=EDGE_CURVE('',#5236,#5237,#2521,.T.);
#6594=EDGE_CURVE('',#5237,#5155,#3060,.T.);
#6595=EDGE_CURVE('',#5235,#5166,#2522,.T.);
#6596=EDGE_CURVE('',#5125,#5107,#3061,.T.);
#6597=EDGE_CURVE('',#5238,#5200,#3062,.T.);
#6598=EDGE_CURVE('',#5238,#5239,#3063,.T.);
#6599=EDGE_CURVE('',#5239,#5201,#3064,.T.);
#6600=EDGE_CURVE('',#5169,#5238,#2523,.T.);
#6601=EDGE_CURVE('',#5240,#5199,#3065,.T.);
#6602=EDGE_CURVE('',#5106,#5240,#3066,.T.);
#6603=EDGE_CURVE('',#5241,#5198,#3067,.T.);
#6604=EDGE_CURVE('',#5240,#5241,#2524,.T.);
#6605=EDGE_CURVE('',#5241,#5126,#3068,.T.);
#6606=EDGE_CURVE('',#5239,#5168,#2525,.T.);
#6607=EDGE_CURVE('',#5141,#5105,#3069,.T.);
#6608=EDGE_CURVE('',#5242,#5204,#3070,.T.);
#6609=EDGE_CURVE('',#5242,#5243,#3071,.T.);
#6610=EDGE_CURVE('',#5243,#5205,#3072,.T.);
#6611=EDGE_CURVE('',#5171,#5242,#2526,.T.);
#6612=EDGE_CURVE('',#5244,#5203,#3073,.T.);
#6613=EDGE_CURVE('',#5104,#5244,#3074,.T.);
#6614=EDGE_CURVE('',#5245,#5202,#3075,.T.);
#6615=EDGE_CURVE('',#5244,#5245,#2527,.T.);
#6616=EDGE_CURVE('',#5245,#5143,#3076,.T.);
#6617=EDGE_CURVE('',#5243,#5170,#2528,.T.);
#6618=EDGE_CURVE('',#5137,#5103,#3077,.T.);
#6619=EDGE_CURVE('',#5246,#5208,#3078,.T.);
#6620=EDGE_CURVE('',#5246,#5247,#3079,.T.);
#6621=EDGE_CURVE('',#5247,#5209,#3080,.T.);
#6622=EDGE_CURVE('',#5173,#5246,#2529,.T.);
#6623=EDGE_CURVE('',#5248,#5207,#3081,.T.);
#6624=EDGE_CURVE('',#5102,#5248,#3082,.T.);
#6625=EDGE_CURVE('',#5249,#5206,#3083,.T.);
#6626=EDGE_CURVE('',#5248,#5249,#2530,.T.);
#6627=EDGE_CURVE('',#5249,#5139,#3084,.T.);
#6628=EDGE_CURVE('',#5247,#5172,#2531,.T.);
#6629=EDGE_CURVE('',#5133,#5101,#3085,.T.);
#6630=EDGE_CURVE('',#5250,#5212,#3086,.T.);
#6631=EDGE_CURVE('',#5250,#5251,#3087,.T.);
#6632=EDGE_CURVE('',#5251,#5213,#3088,.T.);
#6633=EDGE_CURVE('',#5175,#5250,#2532,.T.);
#6634=EDGE_CURVE('',#5252,#5211,#3089,.T.);
#6635=EDGE_CURVE('',#5100,#5252,#3090,.T.);
#6636=EDGE_CURVE('',#5253,#5210,#3091,.T.);
#6637=EDGE_CURVE('',#5252,#5253,#2533,.T.);
#6638=EDGE_CURVE('',#5253,#5135,#3092,.T.);
#6639=EDGE_CURVE('',#5251,#5174,#2534,.T.);
#6640=EDGE_CURVE('',#5129,#5099,#3093,.T.);
#6641=EDGE_CURVE('',#5254,#5216,#3094,.T.);
#6642=EDGE_CURVE('',#5254,#5255,#3095,.T.);
#6643=EDGE_CURVE('',#5255,#5217,#3096,.T.);
#6644=EDGE_CURVE('',#5177,#5254,#2535,.T.);
#6645=EDGE_CURVE('',#5256,#5215,#3097,.T.);
#6646=EDGE_CURVE('',#5098,#5256,#3098,.T.);
#6647=EDGE_CURVE('',#5257,#5214,#3099,.T.);
#6648=EDGE_CURVE('',#5256,#5257,#2536,.T.);
#6649=EDGE_CURVE('',#5257,#5131,#3100,.T.);
#6650=EDGE_CURVE('',#5255,#5176,#2537,.T.);
#6651=EDGE_CURVE('',#5120,#5097,#3101,.T.);
#6652=EDGE_CURVE('',#5258,#5220,#3102,.T.);
#6653=EDGE_CURVE('',#5258,#5259,#3103,.T.);
#6654=EDGE_CURVE('',#5259,#5221,#3104,.T.);
#6655=EDGE_CURVE('',#5179,#5258,#2538,.T.);
#6656=EDGE_CURVE('',#5260,#5219,#3105,.T.);
#6657=EDGE_CURVE('',#5116,#5260,#3106,.T.);
#6658=EDGE_CURVE('',#5261,#5218,#3107,.T.);
#6659=EDGE_CURVE('',#5260,#5261,#2539,.T.);
#6660=EDGE_CURVE('',#5261,#5123,#3108,.T.);
#6661=EDGE_CURVE('',#5259,#5178,#2540,.T.);
#6662=EDGE_CURVE('',#5149,#5115,#3109,.T.);
#6663=EDGE_CURVE('',#5262,#5184,#3110,.T.);
#6664=EDGE_CURVE('',#5262,#5263,#3111,.T.);
#6665=EDGE_CURVE('',#5263,#5185,#3112,.T.);
#6666=EDGE_CURVE('',#5181,#5262,#2541,.T.);
#6667=EDGE_CURVE('',#5264,#5183,#3113,.T.);
#6668=EDGE_CURVE('',#5114,#5264,#3114,.T.);
#6669=EDGE_CURVE('',#5265,#5182,#3115,.T.);
#6670=EDGE_CURVE('',#5264,#5265,#2542,.T.);
#6671=EDGE_CURVE('',#5265,#5151,#3116,.T.);
#6672=EDGE_CURVE('',#5263,#5180,#2543,.T.);
#6673=EDGE_CURVE('',#5145,#5113,#3117,.T.);
#6674=EDGE_CURVE('',#5222,#5224,#3118,.T.);
#6675=EDGE_CURVE('',#5223,#5225,#3119,.T.);
#6676=EDGE_CURVE('',#5266,#5266,#2544,.T.);
#6677=EDGE_CURVE('',#5266,#5267,#2545,.T.);
#6678=EDGE_CURVE('',#5268,#5267,#2546,.T.);
#6679=EDGE_CURVE('',#5267,#5268,#2547,.T.);
#6680=EDGE_CURVE('',#5269,#5270,#2548,.T.);
#6681=EDGE_CURVE('',#5270,#5269,#2549,.T.);
#6682=EDGE_CURVE('',#5270,#5271,#2550,.T.);
#6683=EDGE_CURVE('',#5271,#5271,#2551,.T.);
#6684=EDGE_CURVE('',#5272,#5272,#2552,.T.);
#6685=EDGE_CURVE('',#5272,#5273,#3120,.T.);
#6686=EDGE_CURVE('',#5273,#5273,#2553,.T.);
#6687=EDGE_CURVE('',#5274,#5274,#2554,.T.);
#6688=EDGE_CURVE('',#5274,#5272,#3121,.T.);
#6689=EDGE_CURVE('',#5275,#5275,#2555,.T.);
#6690=EDGE_CURVE('',#5275,#5276,#3122,.T.);
#6691=EDGE_CURVE('',#5276,#5276,#2556,.T.);
#6692=EDGE_CURVE('',#5277,#5277,#2557,.T.);
#6693=EDGE_CURVE('',#5277,#5275,#3123,.T.);
#6694=EDGE_CURVE('',#5278,#5278,#2558,.T.);
#6695=EDGE_CURVE('',#5278,#5279,#3124,.T.);
#6696=EDGE_CURVE('',#5279,#5279,#2559,.T.);
#6697=EDGE_CURVE('',#5280,#5280,#2560,.T.);
#6698=EDGE_CURVE('',#5280,#5278,#3125,.T.);
#6699=EDGE_CURVE('',#5281,#5281,#2561,.T.);
#6700=EDGE_CURVE('',#5281,#5282,#3126,.T.);
#6701=EDGE_CURVE('',#5282,#5282,#2562,.T.);
#6702=EDGE_CURVE('',#5283,#5283,#2563,.T.);
#6703=EDGE_CURVE('',#5283,#5281,#3127,.T.);
#6704=EDGE_CURVE('',#5284,#5284,#2564,.T.);
#6705=EDGE_CURVE('',#5284,#5285,#3128,.T.);
#6706=EDGE_CURVE('',#5285,#5285,#2565,.T.);
#6707=EDGE_CURVE('',#5286,#5286,#2566,.T.);
#6708=EDGE_CURVE('',#5286,#5284,#3129,.T.);
#6709=EDGE_CURVE('',#5287,#5287,#2567,.T.);
#6710=EDGE_CURVE('',#5287,#5288,#3130,.T.);
#6711=EDGE_CURVE('',#5288,#5288,#2568,.T.);
#6712=EDGE_CURVE('',#5289,#5289,#2569,.T.);
#6713=EDGE_CURVE('',#5289,#5287,#3131,.T.);
#6714=EDGE_CURVE('',#5290,#5290,#2570,.T.);
#6715=EDGE_CURVE('',#5290,#5291,#3132,.T.);
#6716=EDGE_CURVE('',#5291,#5291,#2571,.T.);
#6717=EDGE_CURVE('',#5269,#5268,#3133,.T.);
#6718=EDGE_CURVE('',#5292,#5293,#3134,.T.);
#6719=EDGE_CURVE('',#5294,#5292,#3135,.T.);
#6720=EDGE_CURVE('',#5295,#5294,#3136,.T.);
#6721=EDGE_CURVE('',#5295,#5293,#3137,.T.);
#6722=EDGE_CURVE('',#5296,#5292,#3138,.T.);
#6723=EDGE_CURVE('',#5297,#5296,#3139,.T.);
#6724=EDGE_CURVE('',#5294,#5297,#3140,.T.);
#6725=EDGE_CURVE('',#5298,#5296,#2572,.T.);
#6726=EDGE_CURVE('',#5299,#5298,#3141,.T.);
#6727=EDGE_CURVE('',#5297,#5299,#2573,.T.);
#6728=EDGE_CURVE('',#5300,#5298,#3142,.T.);
#6729=EDGE_CURVE('',#5301,#5300,#3143,.T.);
#6730=EDGE_CURVE('',#5299,#5301,#3144,.T.);
#6731=EDGE_CURVE('',#5302,#5300,#2574,.T.);
#6732=EDGE_CURVE('',#5303,#5302,#3145,.T.);
#6733=EDGE_CURVE('',#5301,#5303,#2575,.T.);
#6734=EDGE_CURVE('',#5304,#5302,#3146,.T.);
#6735=EDGE_CURVE('',#5305,#5304,#3147,.T.);
#6736=EDGE_CURVE('',#5303,#5305,#3148,.T.);
#6737=EDGE_CURVE('',#5306,#5304,#2576,.T.);
#6738=EDGE_CURVE('',#5307,#5306,#3149,.T.);
#6739=EDGE_CURVE('',#5305,#5307,#2577,.T.);
#6740=EDGE_CURVE('',#5308,#5306,#3150,.T.);
#6741=EDGE_CURVE('',#5309,#5308,#3151,.T.);
#6742=EDGE_CURVE('',#5307,#5309,#3152,.T.);
#6743=EDGE_CURVE('',#5310,#5308,#2578,.T.);
#6744=EDGE_CURVE('',#5311,#5310,#3153,.T.);
#6745=EDGE_CURVE('',#5309,#5311,#2579,.T.);
#6746=EDGE_CURVE('',#5312,#5310,#3154,.T.);
#6747=EDGE_CURVE('',#5313,#5312,#3155,.T.);
#6748=EDGE_CURVE('',#5311,#5313,#3156,.T.);
#6749=EDGE_CURVE('',#5314,#5312,#3157,.T.);
#6750=EDGE_CURVE('',#5315,#5314,#3158,.T.);
#6751=EDGE_CURVE('',#5313,#5315,#3159,.T.);
#6752=EDGE_CURVE('',#5293,#5314,#3160,.T.);
#6753=EDGE_CURVE('',#5315,#5295,#3161,.T.);
#6754=EDGE_CURVE('',#5316,#5317,#3162,.T.);
#6755=EDGE_CURVE('',#5317,#5318,#2580,.T.);
#6756=EDGE_CURVE('',#5318,#5319,#3163,.T.);
#6757=EDGE_CURVE('',#5319,#5320,#2581,.T.);
#6758=EDGE_CURVE('',#5320,#5321,#3164,.T.);
#6759=EDGE_CURVE('',#5321,#5322,#2582,.T.);
#6760=EDGE_CURVE('',#5322,#5323,#3165,.T.);
#6761=EDGE_CURVE('',#5323,#5324,#2583,.T.);
#6762=EDGE_CURVE('',#5324,#5325,#3166,.T.);
#6763=EDGE_CURVE('',#5326,#5325,#3167,.T.);
#6764=EDGE_CURVE('',#5326,#5327,#3168,.T.);
#6765=EDGE_CURVE('',#5327,#5316,#3169,.T.);
#6766=EDGE_CURVE('',#5326,#5328,#3170,.T.);
#6767=EDGE_CURVE('',#5328,#5329,#3171,.T.);
#6768=EDGE_CURVE('',#5327,#5329,#3172,.T.);
#6769=EDGE_CURVE('',#5325,#5330,#3173,.T.);
#6770=EDGE_CURVE('',#5330,#5328,#3174,.T.);
#6771=EDGE_CURVE('',#5324,#5331,#3175,.T.);
#6772=EDGE_CURVE('',#5331,#5330,#3176,.T.);
#6773=EDGE_CURVE('',#5323,#5332,#3177,.T.);
#6774=EDGE_CURVE('',#5332,#5331,#133,.T.);
#6775=EDGE_CURVE('',#5322,#5333,#3178,.T.);
#6776=EDGE_CURVE('',#5333,#5332,#3179,.T.);
#6777=EDGE_CURVE('',#5321,#5334,#3180,.T.);
#6778=EDGE_CURVE('',#5334,#5333,#134,.T.);
#6779=EDGE_CURVE('',#5320,#5335,#3181,.T.);
#6780=EDGE_CURVE('',#5335,#5334,#3182,.T.);
#6781=EDGE_CURVE('',#5319,#5336,#3183,.T.);
#6782=EDGE_CURVE('',#5336,#5335,#135,.T.);
#6783=EDGE_CURVE('',#5318,#5337,#3184,.T.);
#6784=EDGE_CURVE('',#5337,#5336,#3185,.T.);
#6785=EDGE_CURVE('',#5317,#5338,#3186,.T.);
#6786=EDGE_CURVE('',#5338,#5337,#136,.T.);
#6787=EDGE_CURVE('',#5316,#5339,#3187,.T.);
#6788=EDGE_CURVE('',#5339,#5338,#3188,.T.);
#6789=EDGE_CURVE('',#5329,#5339,#3189,.T.);
#6790=EDGE_CURVE('',#5340,#5341,#3190,.T.);
#6791=EDGE_CURVE('',#5341,#5342,#3191,.T.);
#6792=EDGE_CURVE('',#5342,#5343,#3192,.T.);
#6793=EDGE_CURVE('',#5343,#5344,#3193,.T.);
#6794=EDGE_CURVE('',#5344,#5345,#3194,.T.);
#6795=EDGE_CURVE('',#5345,#5346,#137,.T.);
#6796=EDGE_CURVE('',#5346,#5347,#3195,.T.);
#6797=EDGE_CURVE('',#5347,#5348,#138,.T.);
#6798=EDGE_CURVE('',#5348,#5349,#3196,.T.);
#6799=EDGE_CURVE('',#5349,#5350,#139,.T.);
#6800=EDGE_CURVE('',#5350,#5351,#3197,.T.);
#6801=EDGE_CURVE('',#5351,#5340,#140,.T.);
#6802=EDGE_CURVE('',#5352,#5342,#3198,.T.);
#6803=EDGE_CURVE('',#5352,#5353,#3199,.T.);
#6804=EDGE_CURVE('',#5353,#5343,#3200,.T.);
#6805=EDGE_CURVE('',#5353,#5354,#3201,.T.);
#6806=EDGE_CURVE('',#5354,#5344,#3202,.T.);
#6807=EDGE_CURVE('',#5354,#5355,#3203,.T.);
#6808=EDGE_CURVE('',#5355,#5345,#3204,.T.);
#6809=EDGE_CURVE('',#5355,#5356,#141,.T.);
#6810=EDGE_CURVE('',#5356,#5346,#3205,.T.);
#6811=EDGE_CURVE('',#5356,#5357,#3206,.T.);
#6812=EDGE_CURVE('',#5357,#5347,#3207,.T.);
#6813=EDGE_CURVE('',#5357,#5358,#142,.T.);
#6814=EDGE_CURVE('',#5358,#5348,#3208,.T.);
#6815=EDGE_CURVE('',#5358,#5359,#3209,.T.);
#6816=EDGE_CURVE('',#5359,#5349,#3210,.T.);
#6817=EDGE_CURVE('',#5359,#5360,#143,.T.);
#6818=EDGE_CURVE('',#5360,#5350,#3211,.T.);
#6819=EDGE_CURVE('',#5360,#5361,#3212,.T.);
#6820=EDGE_CURVE('',#5361,#5351,#3213,.T.);
#6821=EDGE_CURVE('',#5361,#5362,#144,.T.);
#6822=EDGE_CURVE('',#5362,#5340,#3214,.T.);
#6823=EDGE_CURVE('',#5362,#5363,#3215,.T.);
#6824=EDGE_CURVE('',#5363,#5341,#3216,.T.);
#6825=EDGE_CURVE('',#5363,#5352,#3217,.T.);
#6826=EDGE_CURVE('',#5364,#5365,#3218,.T.);
#6827=EDGE_CURVE('',#5365,#5366,#3219,.T.);
#6828=EDGE_CURVE('',#5367,#5366,#3220,.T.);
#6829=EDGE_CURVE('',#5364,#5367,#3221,.T.);
#6830=EDGE_CURVE('',#5364,#5368,#3222,.T.);
#6831=EDGE_CURVE('',#5369,#5367,#3223,.T.);
#6832=EDGE_CURVE('',#5368,#5369,#3224,.T.);
#6833=EDGE_CURVE('',#5368,#5370,#2584,.T.);
#6834=EDGE_CURVE('',#5371,#5369,#145,.T.);
#6835=EDGE_CURVE('',#5370,#5371,#3225,.T.);
#6836=EDGE_CURVE('',#5370,#5372,#3226,.T.);
#6837=EDGE_CURVE('',#5373,#5371,#3227,.T.);
#6838=EDGE_CURVE('',#5372,#5373,#3228,.T.);
#6839=EDGE_CURVE('',#5372,#5374,#2585,.T.);
#6840=EDGE_CURVE('',#5375,#5373,#146,.T.);
#6841=EDGE_CURVE('',#5374,#5375,#3229,.T.);
#6842=EDGE_CURVE('',#5374,#5376,#3230,.T.);
#6843=EDGE_CURVE('',#5377,#5375,#3231,.T.);
#6844=EDGE_CURVE('',#5376,#5377,#3232,.T.);
#6845=EDGE_CURVE('',#5376,#5378,#2586,.T.);
#6846=EDGE_CURVE('',#5379,#5377,#147,.T.);
#6847=EDGE_CURVE('',#5378,#5379,#3233,.T.);
#6848=EDGE_CURVE('',#5378,#5380,#3234,.T.);
#6849=EDGE_CURVE('',#5381,#5379,#3235,.T.);
#6850=EDGE_CURVE('',#5380,#5381,#3236,.T.);
#6851=EDGE_CURVE('',#5380,#5382,#2587,.T.);
#6852=EDGE_CURVE('',#5383,#5381,#148,.T.);
#6853=EDGE_CURVE('',#5382,#5383,#3237,.T.);
#6854=EDGE_CURVE('',#5382,#5384,#3238,.T.);
#6855=EDGE_CURVE('',#5385,#5383,#3239,.T.);
#6856=EDGE_CURVE('',#5384,#5385,#3240,.T.);
#6857=EDGE_CURVE('',#5384,#5386,#3241,.T.);
#6858=EDGE_CURVE('',#5387,#5385,#3242,.T.);
#6859=EDGE_CURVE('',#5386,#5387,#3243,.T.);
#6860=EDGE_CURVE('',#5386,#5365,#3244,.T.);
#6861=EDGE_CURVE('',#5366,#5387,#3245,.T.);
#6862=EDGE_CURVE('',#5388,#5389,#3246,.T.);
#6863=EDGE_CURVE('',#5390,#5388,#3247,.T.);
#6864=EDGE_CURVE('',#5391,#5390,#3248,.T.);
#6865=EDGE_CURVE('',#5391,#5389,#3249,.T.);
#6866=EDGE_CURVE('',#5392,#5388,#3250,.T.);
#6867=EDGE_CURVE('',#5393,#5392,#3251,.T.);
#6868=EDGE_CURVE('',#5390,#5393,#3252,.T.);
#6869=EDGE_CURVE('',#5394,#5392,#2588,.T.);
#6870=EDGE_CURVE('',#5395,#5394,#3253,.T.);
#6871=EDGE_CURVE('',#5393,#5395,#2589,.T.);
#6872=EDGE_CURVE('',#5396,#5394,#3254,.T.);
#6873=EDGE_CURVE('',#5397,#5396,#3255,.T.);
#6874=EDGE_CURVE('',#5395,#5397,#3256,.T.);
#6875=EDGE_CURVE('',#5398,#5396,#2590,.T.);
#6876=EDGE_CURVE('',#5399,#5398,#3257,.T.);
#6877=EDGE_CURVE('',#5397,#5399,#2591,.T.);
#6878=EDGE_CURVE('',#5400,#5398,#3258,.T.);
#6879=EDGE_CURVE('',#5401,#5400,#3259,.T.);
#6880=EDGE_CURVE('',#5399,#5401,#3260,.T.);
#6881=EDGE_CURVE('',#5402,#5400,#2592,.T.);
#6882=EDGE_CURVE('',#5403,#5402,#3261,.T.);
#6883=EDGE_CURVE('',#5401,#5403,#2593,.T.);
#6884=EDGE_CURVE('',#5404,#5402,#3262,.T.);
#6885=EDGE_CURVE('',#5405,#5404,#3263,.T.);
#6886=EDGE_CURVE('',#5403,#5405,#3264,.T.);
#6887=EDGE_CURVE('',#5406,#5404,#2594,.T.);
#6888=EDGE_CURVE('',#5407,#5406,#3265,.T.);
#6889=EDGE_CURVE('',#5405,#5407,#2595,.T.);
#6890=EDGE_CURVE('',#5408,#5406,#3266,.T.);
#6891=EDGE_CURVE('',#5409,#5408,#3267,.T.);
#6892=EDGE_CURVE('',#5407,#5409,#3268,.T.);
#6893=EDGE_CURVE('',#5410,#5408,#3269,.T.);
#6894=EDGE_CURVE('',#5411,#5410,#3270,.T.);
#6895=EDGE_CURVE('',#5409,#5411,#3271,.T.);
#6896=EDGE_CURVE('',#5389,#5410,#3272,.T.);
#6897=EDGE_CURVE('',#5411,#5391,#3273,.T.);
#6898=EDGE_CURVE('',#5412,#5413,#3274,.T.);
#6899=EDGE_CURVE('',#5413,#5414,#3275,.T.);
#6900=EDGE_CURVE('',#5414,#5415,#3276,.T.);
#6901=EDGE_CURVE('',#5416,#5415,#3277,.T.);
#6902=EDGE_CURVE('',#5416,#5417,#3278,.T.);
#6903=EDGE_CURVE('',#5417,#5418,#2596,.T.);
#6904=EDGE_CURVE('',#5418,#5419,#3279,.T.);
#6905=EDGE_CURVE('',#5419,#5420,#2597,.T.);
#6906=EDGE_CURVE('',#5420,#5421,#3280,.T.);
#6907=EDGE_CURVE('',#5421,#5422,#2598,.T.);
#6908=EDGE_CURVE('',#5422,#5423,#3281,.T.);
#6909=EDGE_CURVE('',#5423,#5412,#2599,.T.);
#6910=EDGE_CURVE('',#5424,#5414,#3282,.T.);
#6911=EDGE_CURVE('',#5424,#5425,#3283,.T.);
#6912=EDGE_CURVE('',#5425,#5415,#3284,.T.);
#6913=EDGE_CURVE('',#5425,#5426,#3285,.T.);
#6914=EDGE_CURVE('',#5426,#5416,#3286,.T.);
#6915=EDGE_CURVE('',#5426,#5427,#3287,.T.);
#6916=EDGE_CURVE('',#5427,#5417,#3288,.T.);
#6917=EDGE_CURVE('',#5427,#5428,#149,.T.);
#6918=EDGE_CURVE('',#5428,#5418,#3289,.T.);
#6919=EDGE_CURVE('',#5428,#5429,#3290,.T.);
#6920=EDGE_CURVE('',#5429,#5419,#3291,.T.);
#6921=EDGE_CURVE('',#5429,#5430,#150,.T.);
#6922=EDGE_CURVE('',#5430,#5420,#3292,.T.);
#6923=EDGE_CURVE('',#5430,#5431,#3293,.T.);
#6924=EDGE_CURVE('',#5431,#5421,#3294,.T.);
#6925=EDGE_CURVE('',#5431,#5432,#151,.T.);
#6926=EDGE_CURVE('',#5432,#5422,#3295,.T.);
#6927=EDGE_CURVE('',#5432,#5433,#3296,.T.);
#6928=EDGE_CURVE('',#5433,#5423,#3297,.T.);
#6929=EDGE_CURVE('',#5433,#5434,#152,.T.);
#6930=EDGE_CURVE('',#5434,#5412,#3298,.T.);
#6931=EDGE_CURVE('',#5434,#5435,#3299,.T.);
#6932=EDGE_CURVE('',#5435,#5413,#3300,.T.);
#6933=EDGE_CURVE('',#5435,#5424,#3301,.T.);
#6934=EDGE_CURVE('',#5436,#5437,#3302,.T.);
#6935=EDGE_CURVE('',#5438,#5436,#3303,.T.);
#6936=EDGE_CURVE('',#5439,#5438,#3304,.T.);
#6937=EDGE_CURVE('',#5439,#5437,#3305,.T.);
#6938=EDGE_CURVE('',#5440,#5436,#3306,.T.);
#6939=EDGE_CURVE('',#5441,#5440,#3307,.T.);
#6940=EDGE_CURVE('',#5438,#5441,#3308,.T.);
#6941=EDGE_CURVE('',#5442,#5440,#153,.T.);
#6942=EDGE_CURVE('',#5443,#5442,#3309,.T.);
#6943=EDGE_CURVE('',#5441,#5443,#2600,.T.);
#6944=EDGE_CURVE('',#5444,#5442,#3310,.T.);
#6945=EDGE_CURVE('',#5445,#5444,#3311,.T.);
#6946=EDGE_CURVE('',#5443,#5445,#3312,.T.);
#6947=EDGE_CURVE('',#5446,#5444,#154,.T.);
#6948=EDGE_CURVE('',#5447,#5446,#3313,.T.);
#6949=EDGE_CURVE('',#5445,#5447,#2601,.T.);
#6950=EDGE_CURVE('',#5448,#5446,#3314,.T.);
#6951=EDGE_CURVE('',#5449,#5448,#3315,.T.);
#6952=EDGE_CURVE('',#5447,#5449,#3316,.T.);
#6953=EDGE_CURVE('',#5450,#5448,#155,.T.);
#6954=EDGE_CURVE('',#5451,#5450,#3317,.T.);
#6955=EDGE_CURVE('',#5449,#5451,#2602,.T.);
#6956=EDGE_CURVE('',#5452,#5450,#3318,.T.);
#6957=EDGE_CURVE('',#5453,#5452,#3319,.T.);
#6958=EDGE_CURVE('',#5451,#5453,#3320,.T.);
#6959=EDGE_CURVE('',#5454,#5452,#156,.T.);
#6960=EDGE_CURVE('',#5455,#5454,#3321,.T.);
#6961=EDGE_CURVE('',#5453,#5455,#2603,.T.);
#6962=EDGE_CURVE('',#5456,#5454,#3322,.T.);
#6963=EDGE_CURVE('',#5457,#5456,#3323,.T.);
#6964=EDGE_CURVE('',#5455,#5457,#3324,.T.);
#6965=EDGE_CURVE('',#5458,#5456,#3325,.T.);
#6966=EDGE_CURVE('',#5459,#5458,#3326,.T.);
#6967=EDGE_CURVE('',#5459,#5457,#3327,.T.);
#6968=EDGE_CURVE('',#5437,#5458,#3328,.T.);
#6969=EDGE_CURVE('',#5459,#5439,#3329,.T.);
#6970=EDGE_CURVE('',#5460,#5461,#3330,.T.);
#6971=EDGE_CURVE('',#5461,#5462,#3331,.T.);
#6972=EDGE_CURVE('',#5462,#5463,#3332,.T.);
#6973=EDGE_CURVE('',#5463,#5464,#3333,.T.);
#6974=EDGE_CURVE('',#5464,#5465,#3334,.T.);
#6975=EDGE_CURVE('',#5465,#5466,#157,.T.);
#6976=EDGE_CURVE('',#5466,#5467,#3335,.T.);
#6977=EDGE_CURVE('',#5467,#5468,#158,.T.);
#6978=EDGE_CURVE('',#5468,#5469,#3336,.T.);
#6979=EDGE_CURVE('',#5469,#5470,#159,.T.);
#6980=EDGE_CURVE('',#5470,#5471,#3337,.T.);
#6981=EDGE_CURVE('',#5471,#5460,#160,.T.);
#6982=EDGE_CURVE('',#5472,#5462,#3338,.T.);
#6983=EDGE_CURVE('',#5472,#5473,#3339,.T.);
#6984=EDGE_CURVE('',#5473,#5463,#3340,.T.);
#6985=EDGE_CURVE('',#5473,#5474,#3341,.T.);
#6986=EDGE_CURVE('',#5474,#5464,#3342,.T.);
#6987=EDGE_CURVE('',#5474,#5475,#3343,.T.);
#6988=EDGE_CURVE('',#5475,#5465,#3344,.T.);
#6989=EDGE_CURVE('',#5475,#5476,#161,.T.);
#6990=EDGE_CURVE('',#5476,#5466,#3345,.T.);
#6991=EDGE_CURVE('',#5476,#5477,#3346,.T.);
#6992=EDGE_CURVE('',#5477,#5467,#3347,.T.);
#6993=EDGE_CURVE('',#5477,#5478,#162,.T.);
#6994=EDGE_CURVE('',#5478,#5468,#3348,.T.);
#6995=EDGE_CURVE('',#5478,#5479,#3349,.T.);
#6996=EDGE_CURVE('',#5479,#5469,#3350,.T.);
#6997=EDGE_CURVE('',#5479,#5480,#163,.T.);
#6998=EDGE_CURVE('',#5480,#5470,#3351,.T.);
#6999=EDGE_CURVE('',#5480,#5481,#3352,.T.);
#7000=EDGE_CURVE('',#5481,#5471,#3353,.T.);
#7001=EDGE_CURVE('',#5481,#5482,#164,.T.);
#7002=EDGE_CURVE('',#5482,#5460,#3354,.T.);
#7003=EDGE_CURVE('',#5482,#5483,#3355,.T.);
#7004=EDGE_CURVE('',#5483,#5461,#3356,.T.);
#7005=EDGE_CURVE('',#5483,#5472,#3357,.T.);
#7006=EDGE_CURVE('',#5484,#5485,#3358,.T.);
#7007=EDGE_CURVE('',#5485,#5486,#3359,.T.);
#7008=EDGE_CURVE('',#5486,#5487,#2604,.T.);
#7009=EDGE_CURVE('',#5487,#5488,#3360,.T.);
#7010=EDGE_CURVE('',#5488,#5489,#2605,.T.);
#7011=EDGE_CURVE('',#5489,#5490,#3361,.T.);
#7012=EDGE_CURVE('',#5490,#5491,#2606,.T.);
#7013=EDGE_CURVE('',#5491,#5492,#3362,.T.);
#7014=EDGE_CURVE('',#5492,#5493,#2607,.T.);
#7015=EDGE_CURVE('',#5493,#5494,#3363,.T.);
#7016=EDGE_CURVE('',#5494,#5495,#3364,.T.);
#7017=EDGE_CURVE('',#5495,#5484,#3365,.T.);
#7018=EDGE_CURVE('',#5495,#5496,#3366,.T.);
#7019=EDGE_CURVE('',#5496,#5497,#3367,.T.);
#7020=EDGE_CURVE('',#5484,#5497,#3368,.T.);
#7021=EDGE_CURVE('',#5494,#5498,#3369,.T.);
#7022=EDGE_CURVE('',#5498,#5496,#3370,.T.);
#7023=EDGE_CURVE('',#5493,#5499,#3371,.T.);
#7024=EDGE_CURVE('',#5499,#5498,#3372,.T.);
#7025=EDGE_CURVE('',#5492,#5500,#3373,.T.);
#7026=EDGE_CURVE('',#5500,#5499,#165,.T.);
#7027=EDGE_CURVE('',#5491,#5501,#3374,.T.);
#7028=EDGE_CURVE('',#5501,#5500,#3375,.T.);
#7029=EDGE_CURVE('',#5490,#5502,#3376,.T.);
#7030=EDGE_CURVE('',#5502,#5501,#166,.T.);
#7031=EDGE_CURVE('',#5489,#5503,#3377,.T.);
#7032=EDGE_CURVE('',#5503,#5502,#3378,.T.);
#7033=EDGE_CURVE('',#5488,#5504,#3379,.T.);
#7034=EDGE_CURVE('',#5504,#5503,#167,.T.);
#7035=EDGE_CURVE('',#5487,#5505,#3380,.T.);
#7036=EDGE_CURVE('',#5505,#5504,#3381,.T.);
#7037=EDGE_CURVE('',#5486,#5506,#3382,.T.);
#7038=EDGE_CURVE('',#5506,#5505,#168,.T.);
#7039=EDGE_CURVE('',#5485,#5507,#3383,.T.);
#7040=EDGE_CURVE('',#5507,#5506,#3384,.T.);
#7041=EDGE_CURVE('',#5497,#5507,#3385,.T.);
#7042=EDGE_CURVE('',#5508,#5509,#3386,.T.);
#7043=EDGE_CURVE('',#5510,#5508,#3387,.T.);
#7044=EDGE_CURVE('',#5511,#5510,#3388,.T.);
#7045=EDGE_CURVE('',#5512,#5511,#3389,.T.);
#7046=EDGE_CURVE('',#5513,#5512,#2608,.T.);
#7047=EDGE_CURVE('',#5514,#5513,#3390,.T.);
#7048=EDGE_CURVE('',#5515,#5514,#2609,.T.);
#7049=EDGE_CURVE('',#5516,#5515,#3391,.T.);
#7050=EDGE_CURVE('',#5517,#5516,#2610,.T.);
#7051=EDGE_CURVE('',#5518,#5517,#3392,.T.);
#7052=EDGE_CURVE('',#5519,#5518,#2611,.T.);
#7053=EDGE_CURVE('',#5509,#5519,#3393,.T.);
#7054=EDGE_CURVE('',#5520,#5508,#3394,.T.);
#7055=EDGE_CURVE('',#5520,#5521,#3395,.T.);
#7056=EDGE_CURVE('',#5521,#5510,#3396,.T.);
#7057=EDGE_CURVE('',#5521,#5522,#3397,.T.);
#7058=EDGE_CURVE('',#5522,#5511,#3398,.T.);
#7059=EDGE_CURVE('',#5522,#5523,#3399,.T.);
#7060=EDGE_CURVE('',#5523,#5512,#3400,.T.);
#7061=EDGE_CURVE('',#5523,#5524,#169,.T.);
#7062=EDGE_CURVE('',#5524,#5513,#3401,.T.);
#7063=EDGE_CURVE('',#5524,#5525,#3402,.T.);
#7064=EDGE_CURVE('',#5525,#5514,#3403,.T.);
#7065=EDGE_CURVE('',#5525,#5526,#170,.T.);
#7066=EDGE_CURVE('',#5526,#5515,#3404,.T.);
#7067=EDGE_CURVE('',#5526,#5527,#3405,.T.);
#7068=EDGE_CURVE('',#5527,#5516,#3406,.T.);
#7069=EDGE_CURVE('',#5527,#5528,#171,.T.);
#7070=EDGE_CURVE('',#5528,#5517,#3407,.T.);
#7071=EDGE_CURVE('',#5528,#5529,#3408,.T.);
#7072=EDGE_CURVE('',#5529,#5518,#3409,.T.);
#7073=EDGE_CURVE('',#5529,#5530,#172,.T.);
#7074=EDGE_CURVE('',#5530,#5519,#3410,.T.);
#7075=EDGE_CURVE('',#5530,#5531,#3411,.T.);
#7076=EDGE_CURVE('',#5531,#5509,#3412,.T.);
#7077=EDGE_CURVE('',#5531,#5520,#3413,.T.);
#7078=EDGE_CURVE('',#5532,#5533,#3414,.T.);
#7079=EDGE_CURVE('',#5534,#5533,#3415,.T.);
#7080=EDGE_CURVE('',#5535,#5534,#3416,.T.);
#7081=EDGE_CURVE('',#5535,#5532,#3417,.T.);
#7082=EDGE_CURVE('',#5533,#5536,#3418,.T.);
#7083=EDGE_CURVE('',#5537,#5536,#3419,.T.);
#7084=EDGE_CURVE('',#5534,#5537,#3420,.T.);
#7085=EDGE_CURVE('',#5536,#5538,#2612,.T.);
#7086=EDGE_CURVE('',#5539,#5538,#3421,.T.);
#7087=EDGE_CURVE('',#5537,#5539,#2613,.T.);
#7088=EDGE_CURVE('',#5538,#5540,#3422,.T.);
#7089=EDGE_CURVE('',#5541,#5540,#3423,.T.);
#7090=EDGE_CURVE('',#5539,#5541,#3424,.T.);
#7091=EDGE_CURVE('',#5540,#5542,#2614,.T.);
#7092=EDGE_CURVE('',#5543,#5542,#3425,.T.);
#7093=EDGE_CURVE('',#5541,#5543,#2615,.T.);
#7094=EDGE_CURVE('',#5542,#5544,#3426,.T.);
#7095=EDGE_CURVE('',#5545,#5544,#3427,.T.);
#7096=EDGE_CURVE('',#5543,#5545,#3428,.T.);
#7097=EDGE_CURVE('',#5544,#5546,#2616,.T.);
#7098=EDGE_CURVE('',#5547,#5546,#3429,.T.);
#7099=EDGE_CURVE('',#5545,#5547,#2617,.T.);
#7100=EDGE_CURVE('',#5546,#5548,#3430,.T.);
#7101=EDGE_CURVE('',#5549,#5548,#3431,.T.);
#7102=EDGE_CURVE('',#5547,#5549,#3432,.T.);
#7103=EDGE_CURVE('',#5548,#5532,#3433,.T.);
#7104=EDGE_CURVE('',#5549,#5535,#3434,.T.);
#7105=EDGE_CURVE('',#5550,#5551,#3435,.T.);
#7106=EDGE_CURVE('',#5552,#5551,#3436,.T.);
#7107=EDGE_CURVE('',#5553,#5552,#3437,.T.);
#7108=EDGE_CURVE('',#5553,#5550,#3438,.T.);
#7109=EDGE_CURVE('',#5551,#5554,#3439,.T.);
#7110=EDGE_CURVE('',#5555,#5554,#3440,.T.);
#7111=EDGE_CURVE('',#5552,#5555,#3441,.T.);
#7112=EDGE_CURVE('',#5554,#5556,#2618,.T.);
#7113=EDGE_CURVE('',#5557,#5556,#3442,.T.);
#7114=EDGE_CURVE('',#5555,#5557,#2619,.T.);
#7115=EDGE_CURVE('',#5556,#5558,#3443,.T.);
#7116=EDGE_CURVE('',#5559,#5558,#3444,.T.);
#7117=EDGE_CURVE('',#5557,#5559,#3445,.T.);
#7118=EDGE_CURVE('',#5558,#5560,#2620,.T.);
#7119=EDGE_CURVE('',#5561,#5560,#3446,.T.);
#7120=EDGE_CURVE('',#5559,#5561,#2621,.T.);
#7121=EDGE_CURVE('',#5560,#5562,#3447,.T.);
#7122=EDGE_CURVE('',#5563,#5562,#3448,.T.);
#7123=EDGE_CURVE('',#5561,#5563,#3449,.T.);
#7124=EDGE_CURVE('',#5562,#5564,#2622,.T.);
#7125=EDGE_CURVE('',#5565,#5564,#3450,.T.);
#7126=EDGE_CURVE('',#5563,#5565,#2623,.T.);
#7127=EDGE_CURVE('',#5564,#5566,#3451,.T.);
#7128=EDGE_CURVE('',#5567,#5566,#3452,.T.);
#7129=EDGE_CURVE('',#5565,#5567,#3453,.T.);
#7130=EDGE_CURVE('',#5566,#5550,#3454,.T.);
#7131=EDGE_CURVE('',#5567,#5553,#3455,.T.);
#7132=EDGE_CURVE('',#5568,#5569,#3456,.T.);
#7133=EDGE_CURVE('',#5570,#5568,#3457,.T.);
#7134=EDGE_CURVE('',#5570,#5571,#3458,.T.);
#7135=EDGE_CURVE('',#5571,#5569,#3459,.T.);
#7136=EDGE_CURVE('',#5569,#5572,#3460,.T.);
#7137=EDGE_CURVE('',#5571,#5573,#3461,.T.);
#7138=EDGE_CURVE('',#5573,#5572,#3462,.T.);
#7139=EDGE_CURVE('',#5572,#5574,#2624,.T.);
#7140=EDGE_CURVE('',#5573,#5575,#2625,.T.);
#7141=EDGE_CURVE('',#5575,#5574,#3463,.T.);
#7142=EDGE_CURVE('',#5574,#5576,#3464,.T.);
#7143=EDGE_CURVE('',#5575,#5577,#3465,.T.);
#7144=EDGE_CURVE('',#5577,#5576,#3466,.T.);
#7145=EDGE_CURVE('',#5576,#5578,#2626,.T.);
#7146=EDGE_CURVE('',#5577,#5579,#2627,.T.);
#7147=EDGE_CURVE('',#5579,#5578,#3467,.T.);
#7148=EDGE_CURVE('',#5578,#5580,#3468,.T.);
#7149=EDGE_CURVE('',#5579,#5581,#3469,.T.);
#7150=EDGE_CURVE('',#5581,#5580,#3470,.T.);
#7151=EDGE_CURVE('',#5580,#5582,#2628,.T.);
#7152=EDGE_CURVE('',#5581,#5583,#2629,.T.);
#7153=EDGE_CURVE('',#5583,#5582,#3471,.T.);
#7154=EDGE_CURVE('',#5582,#5584,#3472,.T.);
#7155=EDGE_CURVE('',#5583,#5585,#3473,.T.);
#7156=EDGE_CURVE('',#5585,#5584,#3474,.T.);
#7157=EDGE_CURVE('',#5584,#5568,#3475,.T.);
#7158=EDGE_CURVE('',#5585,#5570,#3476,.T.);
#7159=EDGE_CURVE('',#5586,#5587,#3477,.T.);
#7160=EDGE_CURVE('',#5588,#5586,#3478,.T.);
#7161=EDGE_CURVE('',#5588,#5589,#3479,.T.);
#7162=EDGE_CURVE('',#5589,#5587,#3480,.T.);
#7163=EDGE_CURVE('',#5587,#5590,#3481,.T.);
#7164=EDGE_CURVE('',#5589,#5591,#3482,.T.);
#7165=EDGE_CURVE('',#5591,#5590,#3483,.T.);
#7166=EDGE_CURVE('',#5590,#5592,#2630,.T.);
#7167=EDGE_CURVE('',#5591,#5593,#2631,.T.);
#7168=EDGE_CURVE('',#5593,#5592,#3484,.T.);
#7169=EDGE_CURVE('',#5592,#5594,#3485,.T.);
#7170=EDGE_CURVE('',#5593,#5595,#3486,.T.);
#7171=EDGE_CURVE('',#5595,#5594,#3487,.T.);
#7172=EDGE_CURVE('',#5594,#5596,#2632,.T.);
#7173=EDGE_CURVE('',#5595,#5597,#2633,.T.);
#7174=EDGE_CURVE('',#5597,#5596,#3488,.T.);
#7175=EDGE_CURVE('',#5596,#5598,#3489,.T.);
#7176=EDGE_CURVE('',#5597,#5599,#3490,.T.);
#7177=EDGE_CURVE('',#5599,#5598,#3491,.T.);
#7178=EDGE_CURVE('',#5598,#5600,#2634,.T.);
#7179=EDGE_CURVE('',#5599,#5601,#2635,.T.);
#7180=EDGE_CURVE('',#5601,#5600,#3492,.T.);
#7181=EDGE_CURVE('',#5600,#5602,#3493,.T.);
#7182=EDGE_CURVE('',#5601,#5603,#3494,.T.);
#7183=EDGE_CURVE('',#5603,#5602,#3495,.T.);
#7184=EDGE_CURVE('',#5602,#5586,#3496,.T.);
#7185=EDGE_CURVE('',#5603,#5588,#3497,.T.);
#7186=EDGE_CURVE('',#5604,#5605,#3498,.T.);
#7187=EDGE_CURVE('',#5605,#5606,#3499,.T.);
#7188=EDGE_CURVE('',#5606,#5607,#2636,.T.);
#7189=EDGE_CURVE('',#5607,#5608,#3500,.T.);
#7190=EDGE_CURVE('',#5608,#5609,#2637,.T.);
#7191=EDGE_CURVE('',#5609,#5610,#3501,.T.);
#7192=EDGE_CURVE('',#5610,#5611,#2638,.T.);
#7193=EDGE_CURVE('',#5611,#5612,#3502,.T.);
#7194=EDGE_CURVE('',#5612,#5604,#3503,.T.);
#7195=EDGE_CURVE('',#5612,#5613,#3504,.T.);
#7196=EDGE_CURVE('',#5613,#5614,#3505,.T.);
#7197=EDGE_CURVE('',#5604,#5614,#3506,.T.);
#7198=EDGE_CURVE('',#5611,#5615,#3507,.T.);
#7199=EDGE_CURVE('',#5615,#5613,#3508,.T.);
#7200=EDGE_CURVE('',#5610,#5616,#3509,.T.);
#7201=EDGE_CURVE('',#5616,#5615,#173,.T.);
#7202=EDGE_CURVE('',#5609,#5617,#3510,.T.);
#7203=EDGE_CURVE('',#5617,#5616,#3511,.T.);
#7204=EDGE_CURVE('',#5608,#5618,#3512,.T.);
#7205=EDGE_CURVE('',#5618,#5617,#174,.T.);
#7206=EDGE_CURVE('',#5607,#5619,#3513,.T.);
#7207=EDGE_CURVE('',#5619,#5618,#3514,.T.);
#7208=EDGE_CURVE('',#5606,#5620,#3515,.T.);
#7209=EDGE_CURVE('',#5620,#5619,#175,.T.);
#7210=EDGE_CURVE('',#5605,#5621,#3516,.T.);
#7211=EDGE_CURVE('',#5621,#5620,#3517,.T.);
#7212=EDGE_CURVE('',#5614,#5621,#3518,.T.);
#7213=EDGE_CURVE('',#5622,#5623,#3519,.T.);
#7214=EDGE_CURVE('',#5624,#5622,#3520,.T.);
#7215=EDGE_CURVE('',#5625,#5624,#3521,.T.);
#7216=EDGE_CURVE('',#5625,#5623,#3522,.T.);
#7217=EDGE_CURVE('',#5626,#5622,#3523,.T.);
#7218=EDGE_CURVE('',#5627,#5626,#3524,.T.);
#7219=EDGE_CURVE('',#5624,#5627,#3525,.T.);
#7220=EDGE_CURVE('',#5628,#5626,#176,.T.);
#7221=EDGE_CURVE('',#5629,#5628,#3526,.T.);
#7222=EDGE_CURVE('',#5627,#5629,#177,.T.);
#7223=EDGE_CURVE('',#5630,#5628,#3527,.T.);
#7224=EDGE_CURVE('',#5631,#5630,#3528,.T.);
#7225=EDGE_CURVE('',#5629,#5631,#3529,.T.);
#7226=EDGE_CURVE('',#5632,#5630,#178,.T.);
#7227=EDGE_CURVE('',#5633,#5632,#3530,.T.);
#7228=EDGE_CURVE('',#5631,#5633,#179,.T.);
#7229=EDGE_CURVE('',#5634,#5632,#3531,.T.);
#7230=EDGE_CURVE('',#5635,#5634,#3532,.T.);
#7231=EDGE_CURVE('',#5633,#5635,#3533,.T.);
#7232=EDGE_CURVE('',#5636,#5634,#180,.T.);
#7233=EDGE_CURVE('',#5637,#5636,#3534,.T.);
#7234=EDGE_CURVE('',#5635,#5637,#181,.T.);
#7235=EDGE_CURVE('',#5638,#5636,#3535,.T.);
#7236=EDGE_CURVE('',#5639,#5638,#3536,.T.);
#7237=EDGE_CURVE('',#5637,#5639,#3537,.T.);
#7238=EDGE_CURVE('',#5623,#5638,#3538,.T.);
#7239=EDGE_CURVE('',#5639,#5625,#3539,.T.);
#7240=EDGE_CURVE('',#5640,#5641,#3540,.T.);
#7241=EDGE_CURVE('',#5642,#5640,#3541,.T.);
#7242=EDGE_CURVE('',#5643,#5642,#3542,.T.);
#7243=EDGE_CURVE('',#5644,#5643,#2639,.T.);
#7244=EDGE_CURVE('',#5645,#5644,#3543,.T.);
#7245=EDGE_CURVE('',#5646,#5645,#2640,.T.);
#7246=EDGE_CURVE('',#5647,#5646,#3544,.T.);
#7247=EDGE_CURVE('',#5648,#5647,#2641,.T.);
#7248=EDGE_CURVE('',#5641,#5648,#3545,.T.);
#7249=EDGE_CURVE('',#5649,#5640,#3546,.T.);
#7250=EDGE_CURVE('',#5649,#5650,#3547,.T.);
#7251=EDGE_CURVE('',#5650,#5642,#3548,.T.);
#7252=EDGE_CURVE('',#5650,#5651,#3549,.T.);
#7253=EDGE_CURVE('',#5651,#5643,#3550,.T.);
#7254=EDGE_CURVE('',#5651,#5652,#182,.T.);
#7255=EDGE_CURVE('',#5652,#5644,#3551,.T.);
#7256=EDGE_CURVE('',#5652,#5653,#3552,.T.);
#7257=EDGE_CURVE('',#5653,#5645,#3553,.T.);
#7258=EDGE_CURVE('',#5653,#5654,#183,.T.);
#7259=EDGE_CURVE('',#5654,#5646,#3554,.T.);
#7260=EDGE_CURVE('',#5654,#5655,#3555,.T.);
#7261=EDGE_CURVE('',#5655,#5647,#3556,.T.);
#7262=EDGE_CURVE('',#5655,#5656,#184,.T.);
#7263=EDGE_CURVE('',#5656,#5648,#3557,.T.);
#7264=EDGE_CURVE('',#5656,#5657,#3558,.T.);
#7265=EDGE_CURVE('',#5657,#5641,#3559,.T.);
#7266=EDGE_CURVE('',#5657,#5649,#3560,.T.);
#7267=EDGE_CURVE('',#5658,#5659,#3561,.T.);
#7268=EDGE_CURVE('',#5660,#5658,#3562,.T.);
#7269=EDGE_CURVE('',#5661,#5660,#3563,.T.);
#7270=EDGE_CURVE('',#5662,#5661,#2642,.T.);
#7271=EDGE_CURVE('',#5663,#5662,#3564,.T.);
#7272=EDGE_CURVE('',#5664,#5663,#2643,.T.);
#7273=EDGE_CURVE('',#5665,#5664,#3565,.T.);
#7274=EDGE_CURVE('',#5666,#5665,#2644,.T.);
#7275=EDGE_CURVE('',#5659,#5666,#3566,.T.);
#7276=EDGE_CURVE('',#5667,#5658,#3567,.T.);
#7277=EDGE_CURVE('',#5667,#5668,#3568,.T.);
#7278=EDGE_CURVE('',#5668,#5660,#3569,.T.);
#7279=EDGE_CURVE('',#5668,#5669,#3570,.T.);
#7280=EDGE_CURVE('',#5669,#5661,#3571,.T.);
#7281=EDGE_CURVE('',#5669,#5670,#185,.T.);
#7282=EDGE_CURVE('',#5670,#5662,#3572,.T.);
#7283=EDGE_CURVE('',#5670,#5671,#3573,.T.);
#7284=EDGE_CURVE('',#5671,#5663,#3574,.T.);
#7285=EDGE_CURVE('',#5671,#5672,#186,.T.);
#7286=EDGE_CURVE('',#5672,#5664,#3575,.T.);
#7287=EDGE_CURVE('',#5672,#5673,#3576,.T.);
#7288=EDGE_CURVE('',#5673,#5665,#3577,.T.);
#7289=EDGE_CURVE('',#5673,#5674,#187,.T.);
#7290=EDGE_CURVE('',#5674,#5666,#3578,.T.);
#7291=EDGE_CURVE('',#5674,#5675,#3579,.T.);
#7292=EDGE_CURVE('',#5675,#5659,#3580,.T.);
#7293=EDGE_CURVE('',#5675,#5667,#3581,.T.);
#7294=EDGE_CURVE('',#5676,#5677,#3582,.T.);
#7295=EDGE_CURVE('',#5676,#5678,#3583,.T.);
#7296=EDGE_CURVE('',#5679,#5678,#3584,.T.);
#7297=EDGE_CURVE('',#5677,#5679,#3585,.T.);
#7298=EDGE_CURVE('',#5677,#5680,#3586,.T.);
#7299=EDGE_CURVE('',#5681,#5679,#3587,.T.);
#7300=EDGE_CURVE('',#5680,#5681,#3588,.T.);
#7301=EDGE_CURVE('',#5680,#5682,#188,.T.);
#7302=EDGE_CURVE('',#5683,#5681,#189,.T.);
#7303=EDGE_CURVE('',#5682,#5683,#3589,.T.);
#7304=EDGE_CURVE('',#5682,#5684,#3590,.T.);
#7305=EDGE_CURVE('',#5685,#5683,#3591,.T.);
#7306=EDGE_CURVE('',#5684,#5685,#3592,.T.);
#7307=EDGE_CURVE('',#5684,#5686,#190,.T.);
#7308=EDGE_CURVE('',#5687,#5685,#191,.T.);
#7309=EDGE_CURVE('',#5686,#5687,#3593,.T.);
#7310=EDGE_CURVE('',#5686,#5688,#3594,.T.);
#7311=EDGE_CURVE('',#5689,#5687,#3595,.T.);
#7312=EDGE_CURVE('',#5688,#5689,#3596,.T.);
#7313=EDGE_CURVE('',#5688,#5690,#192,.T.);
#7314=EDGE_CURVE('',#5691,#5689,#193,.T.);
#7315=EDGE_CURVE('',#5690,#5691,#3597,.T.);
#7316=EDGE_CURVE('',#5690,#5692,#3598,.T.);
#7317=EDGE_CURVE('',#5693,#5691,#3599,.T.);
#7318=EDGE_CURVE('',#5692,#5693,#3600,.T.);
#7319=EDGE_CURVE('',#5692,#5676,#3601,.T.);
#7320=EDGE_CURVE('',#5678,#5693,#3602,.T.);
#7321=EDGE_CURVE('',#5694,#5695,#3603,.T.);
#7322=EDGE_CURVE('',#5695,#5696,#3604,.T.);
#7323=EDGE_CURVE('',#5696,#5697,#2645,.T.);
#7324=EDGE_CURVE('',#5697,#5698,#3605,.T.);
#7325=EDGE_CURVE('',#5698,#5699,#2646,.T.);
#7326=EDGE_CURVE('',#5699,#5700,#3606,.T.);
#7327=EDGE_CURVE('',#5700,#5701,#2647,.T.);
#7328=EDGE_CURVE('',#5701,#5702,#3607,.T.);
#7329=EDGE_CURVE('',#5702,#5694,#3608,.T.);
#7330=EDGE_CURVE('',#5702,#5703,#3609,.T.);
#7331=EDGE_CURVE('',#5703,#5704,#3610,.T.);
#7332=EDGE_CURVE('',#5694,#5704,#3611,.T.);
#7333=EDGE_CURVE('',#5701,#5705,#3612,.T.);
#7334=EDGE_CURVE('',#5705,#5703,#3613,.T.);
#7335=EDGE_CURVE('',#5700,#5706,#3614,.T.);
#7336=EDGE_CURVE('',#5706,#5705,#194,.T.);
#7337=EDGE_CURVE('',#5699,#5707,#3615,.T.);
#7338=EDGE_CURVE('',#5707,#5706,#3616,.T.);
#7339=EDGE_CURVE('',#5698,#5708,#3617,.T.);
#7340=EDGE_CURVE('',#5708,#5707,#195,.T.);
#7341=EDGE_CURVE('',#5697,#5709,#3618,.T.);
#7342=EDGE_CURVE('',#5709,#5708,#3619,.T.);
#7343=EDGE_CURVE('',#5696,#5710,#3620,.T.);
#7344=EDGE_CURVE('',#5710,#5709,#196,.T.);
#7345=EDGE_CURVE('',#5695,#5711,#3621,.T.);
#7346=EDGE_CURVE('',#5711,#5710,#3622,.T.);
#7347=EDGE_CURVE('',#5704,#5711,#3623,.T.);
#7348=EDGE_CURVE('',#5712,#5713,#2648,.T.);
#7349=EDGE_CURVE('',#5712,#5714,#3624,.T.);
#7350=EDGE_CURVE('',#5714,#5715,#2649,.T.);
#7351=EDGE_CURVE('',#5713,#5715,#3625,.T.);
#7352=EDGE_CURVE('',#5716,#5717,#2650,.T.);
#7353=EDGE_CURVE('',#5716,#5718,#3626,.T.);
#7354=EDGE_CURVE('',#5718,#5719,#2651,.T.);
#7355=EDGE_CURVE('',#5717,#5719,#3627,.T.);
#7356=EDGE_CURVE('',#5720,#5721,#2652,.T.);
#7357=EDGE_CURVE('',#5720,#5722,#3628,.T.);
#7358=EDGE_CURVE('',#5722,#5723,#2653,.T.);
#7359=EDGE_CURVE('',#5721,#5723,#3629,.T.);
#7360=EDGE_CURVE('',#5724,#5725,#2654,.T.);
#7361=EDGE_CURVE('',#5724,#5726,#3630,.T.);
#7362=EDGE_CURVE('',#5726,#5727,#2655,.T.);
#7363=EDGE_CURVE('',#5725,#5727,#3631,.T.);
#7364=EDGE_CURVE('',#5728,#5729,#3632,.T.);
#7365=EDGE_CURVE('',#5729,#5730,#3633,.T.);
#7366=EDGE_CURVE('',#5731,#5730,#3634,.T.);
#7367=EDGE_CURVE('',#5731,#5728,#3635,.T.);
#7368=EDGE_CURVE('',#5732,#5733,#3636,.T.);
#7369=EDGE_CURVE('',#5732,#5734,#3637,.T.);
#7370=EDGE_CURVE('',#5734,#5735,#3638,.T.);
#7371=EDGE_CURVE('',#5735,#5733,#3639,.T.);
#7372=EDGE_CURVE('',#5736,#5737,#3640,.T.);
#7373=EDGE_CURVE('',#5737,#5738,#3641,.T.);
#7374=EDGE_CURVE('',#5739,#5738,#3642,.T.);
#7375=EDGE_CURVE('',#5739,#5736,#3643,.T.);
#7376=EDGE_CURVE('',#5740,#5741,#3644,.T.);
#7377=EDGE_CURVE('',#5741,#5742,#3645,.T.);
#7378=EDGE_CURVE('',#5743,#5742,#3646,.T.);
#7379=EDGE_CURVE('',#5743,#5740,#3647,.T.);
#7380=EDGE_CURVE('',#5730,#5732,#3648,.T.);
#7381=EDGE_CURVE('',#5733,#5739,#3649,.T.);
#7382=EDGE_CURVE('',#5738,#5743,#3650,.T.);
#7383=EDGE_CURVE('',#5742,#5731,#3651,.T.);
#7384=EDGE_CURVE('',#5715,#5744,#3652,.T.);
#7385=EDGE_CURVE('',#5745,#5714,#3653,.T.);
#7386=EDGE_CURVE('',#5744,#5745,#2656,.T.);
#7387=EDGE_CURVE('',#5719,#5746,#3654,.T.);
#7388=EDGE_CURVE('',#5747,#5718,#3655,.T.);
#7389=EDGE_CURVE('',#5746,#5747,#2657,.T.);
#7390=EDGE_CURVE('',#5723,#5748,#3656,.T.);
#7391=EDGE_CURVE('',#5749,#5722,#3657,.T.);
#7392=EDGE_CURVE('',#5748,#5749,#2658,.T.);
#7393=EDGE_CURVE('',#5727,#5750,#3658,.T.);
#7394=EDGE_CURVE('',#5751,#5726,#3659,.T.);
#7395=EDGE_CURVE('',#5750,#5751,#2659,.T.);
#7396=EDGE_CURVE('',#5734,#5729,#3660,.T.);
#7397=EDGE_CURVE('',#5728,#5741,#3661,.T.);
#7398=EDGE_CURVE('',#5740,#5737,#3662,.T.);
#7399=EDGE_CURVE('',#5736,#5735,#3663,.T.);
#7400=EDGE_CURVE('',#5713,#5752,#3664,.T.);
#7401=EDGE_CURVE('',#5752,#5753,#2660,.T.);
#7402=EDGE_CURVE('',#5753,#5712,#3665,.T.);
#7403=EDGE_CURVE('',#5717,#5754,#3666,.T.);
#7404=EDGE_CURVE('',#5754,#5755,#2661,.T.);
#7405=EDGE_CURVE('',#5755,#5716,#3667,.T.);
#7406=EDGE_CURVE('',#5721,#5756,#3668,.T.);
#7407=EDGE_CURVE('',#5756,#5757,#2662,.T.);
#7408=EDGE_CURVE('',#5757,#5720,#3669,.T.);
#7409=EDGE_CURVE('',#5725,#5758,#3670,.T.);
#7410=EDGE_CURVE('',#5758,#5759,#2663,.T.);
#7411=EDGE_CURVE('',#5759,#5724,#3671,.T.);
#7412=EDGE_CURVE('',#5759,#5751,#3672,.T.);
#7413=EDGE_CURVE('',#5758,#5750,#3673,.T.);
#7414=EDGE_CURVE('',#5757,#5749,#3674,.T.);
#7415=EDGE_CURVE('',#5756,#5748,#3675,.T.);
#7416=EDGE_CURVE('',#5755,#5747,#3676,.T.);
#7417=EDGE_CURVE('',#5754,#5746,#3677,.T.);
#7418=EDGE_CURVE('',#5753,#5745,#3678,.T.);
#7419=EDGE_CURVE('',#5752,#5744,#3679,.T.);
#7420=EDGE_CURVE('',#5760,#5760,#2664,.T.);
#7421=EDGE_CURVE('',#5760,#5761,#3680,.T.);
#7422=EDGE_CURVE('',#5761,#5761,#2665,.T.);
#7423=EDGE_CURVE('',#5762,#5762,#2666,.T.);
#7424=EDGE_CURVE('',#5762,#5763,#3681,.T.);
#7425=EDGE_CURVE('',#5763,#5763,#2667,.T.);
#7426=EDGE_CURVE('',#5764,#5765,#3682,.T.);
#7427=EDGE_CURVE('',#5766,#5764,#3683,.T.);
#7428=EDGE_CURVE('',#5767,#5766,#3684,.T.);
#7429=EDGE_CURVE('',#5767,#5765,#3685,.T.);
#7430=EDGE_CURVE('',#5768,#5764,#3686,.T.);
#7431=EDGE_CURVE('',#5769,#5768,#3687,.T.);
#7432=EDGE_CURVE('',#5766,#5769,#3688,.T.);
#7433=EDGE_CURVE('',#5770,#5768,#197,.T.);
#7434=EDGE_CURVE('',#5771,#5770,#3689,.T.);
#7435=EDGE_CURVE('',#5769,#5771,#198,.T.);
#7436=EDGE_CURVE('',#5772,#5770,#3690,.T.);
#7437=EDGE_CURVE('',#5773,#5772,#3691,.T.);
#7438=EDGE_CURVE('',#5771,#5773,#3692,.T.);
#7439=EDGE_CURVE('',#5774,#5772,#199,.T.);
#7440=EDGE_CURVE('',#5775,#5774,#3693,.T.);
#7441=EDGE_CURVE('',#5773,#5775,#200,.T.);
#7442=EDGE_CURVE('',#5776,#5774,#3694,.T.);
#7443=EDGE_CURVE('',#5777,#5776,#3695,.T.);
#7444=EDGE_CURVE('',#5775,#5777,#3696,.T.);
#7445=EDGE_CURVE('',#5778,#5776,#201,.T.);
#7446=EDGE_CURVE('',#5779,#5778,#3697,.T.);
#7447=EDGE_CURVE('',#5777,#5779,#202,.T.);
#7448=EDGE_CURVE('',#5780,#5778,#3698,.T.);
#7449=EDGE_CURVE('',#5781,#5780,#3699,.T.);
#7450=EDGE_CURVE('',#5779,#5781,#3700,.T.);
#7451=EDGE_CURVE('',#5782,#5780,#203,.T.);
#7452=EDGE_CURVE('',#5783,#5782,#3701,.T.);
#7453=EDGE_CURVE('',#5781,#5783,#204,.T.);
#7454=EDGE_CURVE('',#5784,#5782,#3702,.T.);
#7455=EDGE_CURVE('',#5785,#5784,#3703,.T.);
#7456=EDGE_CURVE('',#5783,#5785,#3704,.T.);
#7457=EDGE_CURVE('',#5786,#5784,#3705,.T.);
#7458=EDGE_CURVE('',#5787,#5786,#3706,.T.);
#7459=EDGE_CURVE('',#5785,#5787,#3707,.T.);
#7460=EDGE_CURVE('',#5765,#5786,#3708,.T.);
#7461=EDGE_CURVE('',#5787,#5767,#3709,.T.);
#7462=EDGE_CURVE('',#5788,#5788,#2668,.T.);
#7463=EDGE_CURVE('',#5788,#5789,#3710,.T.);
#7464=EDGE_CURVE('',#5789,#5789,#2669,.T.);
#7465=EDGE_CURVE('',#5790,#5790,#2670,.T.);
#7466=EDGE_CURVE('',#5790,#5791,#3711,.T.);
#7467=EDGE_CURVE('',#5791,#5791,#2671,.T.);
#7468=EDGE_CURVE('',#5792,#5793,#3712,.T.);
#7469=EDGE_CURVE('',#5794,#5793,#3713,.T.);
#7470=EDGE_CURVE('',#5795,#5794,#3714,.T.);
#7471=EDGE_CURVE('',#5795,#5792,#3715,.T.);
#7472=EDGE_CURVE('',#5793,#5796,#3716,.T.);
#7473=EDGE_CURVE('',#5797,#5796,#3717,.T.);
#7474=EDGE_CURVE('',#5794,#5797,#3718,.T.);
#7475=EDGE_CURVE('',#5796,#5798,#2672,.T.);
#7476=EDGE_CURVE('',#5799,#5798,#3719,.T.);
#7477=EDGE_CURVE('',#5797,#5799,#2673,.T.);
#7478=EDGE_CURVE('',#5798,#5800,#3720,.T.);
#7479=EDGE_CURVE('',#5801,#5800,#3721,.T.);
#7480=EDGE_CURVE('',#5799,#5801,#3722,.T.);
#7481=EDGE_CURVE('',#5800,#5802,#2674,.T.);
#7482=EDGE_CURVE('',#5803,#5802,#3723,.T.);
#7483=EDGE_CURVE('',#5801,#5803,#2675,.T.);
#7484=EDGE_CURVE('',#5802,#5804,#3724,.T.);
#7485=EDGE_CURVE('',#5805,#5804,#3725,.T.);
#7486=EDGE_CURVE('',#5803,#5805,#3726,.T.);
#7487=EDGE_CURVE('',#5804,#5806,#2676,.T.);
#7488=EDGE_CURVE('',#5807,#5806,#3727,.T.);
#7489=EDGE_CURVE('',#5805,#5807,#2677,.T.);
#7490=EDGE_CURVE('',#5806,#5808,#3728,.T.);
#7491=EDGE_CURVE('',#5809,#5808,#3729,.T.);
#7492=EDGE_CURVE('',#5807,#5809,#3730,.T.);
#7493=EDGE_CURVE('',#5808,#5792,#3731,.T.);
#7494=EDGE_CURVE('',#5809,#5795,#3732,.T.);
#7495=EDGE_CURVE('',#5810,#5810,#2678,.T.);
#7496=EDGE_CURVE('',#5810,#5811,#3733,.T.);
#7497=EDGE_CURVE('',#5811,#5811,#2679,.T.);
#7498=EDGE_CURVE('',#5812,#5812,#2680,.T.);
#7499=EDGE_CURVE('',#5812,#5813,#3734,.T.);
#7500=EDGE_CURVE('',#5813,#5813,#2681,.T.);
#7501=EDGE_CURVE('',#5814,#5815,#3735,.T.);
#7502=EDGE_CURVE('',#5816,#5814,#3736,.T.);
#7503=EDGE_CURVE('',#5816,#5817,#3737,.T.);
#7504=EDGE_CURVE('',#5817,#5815,#3738,.T.);
#7505=EDGE_CURVE('',#5815,#5818,#3739,.T.);
#7506=EDGE_CURVE('',#5817,#5819,#3740,.T.);
#7507=EDGE_CURVE('',#5819,#5818,#3741,.T.);
#7508=EDGE_CURVE('',#5818,#5820,#2682,.T.);
#7509=EDGE_CURVE('',#5819,#5821,#2683,.T.);
#7510=EDGE_CURVE('',#5821,#5820,#3742,.T.);
#7511=EDGE_CURVE('',#5820,#5822,#3743,.T.);
#7512=EDGE_CURVE('',#5821,#5823,#3744,.T.);
#7513=EDGE_CURVE('',#5823,#5822,#3745,.T.);
#7514=EDGE_CURVE('',#5822,#5824,#2684,.T.);
#7515=EDGE_CURVE('',#5823,#5825,#2685,.T.);
#7516=EDGE_CURVE('',#5825,#5824,#3746,.T.);
#7517=EDGE_CURVE('',#5824,#5826,#3747,.T.);
#7518=EDGE_CURVE('',#5825,#5827,#3748,.T.);
#7519=EDGE_CURVE('',#5827,#5826,#3749,.T.);
#7520=EDGE_CURVE('',#5826,#5828,#2686,.T.);
#7521=EDGE_CURVE('',#5827,#5829,#2687,.T.);
#7522=EDGE_CURVE('',#5829,#5828,#3750,.T.);
#7523=EDGE_CURVE('',#5828,#5830,#3751,.T.);
#7524=EDGE_CURVE('',#5829,#5831,#3752,.T.);
#7525=EDGE_CURVE('',#5831,#5830,#3753,.T.);
#7526=EDGE_CURVE('',#5830,#5814,#3754,.T.);
#7527=EDGE_CURVE('',#5831,#5816,#3755,.T.);
#7528=ORIENTED_EDGE('',*,*,#5832,.F.);
#7529=ORIENTED_EDGE('',*,*,#5833,.F.);
#7530=ORIENTED_EDGE('',*,*,#5834,.F.);
#7531=ORIENTED_EDGE('',*,*,#5835,.F.);
#7532=ORIENTED_EDGE('',*,*,#5836,.F.);
#7533=ORIENTED_EDGE('',*,*,#5837,.T.);
#7534=ORIENTED_EDGE('',*,*,#5838,.F.);
#7535=ORIENTED_EDGE('',*,*,#5837,.F.);
#7536=ORIENTED_EDGE('',*,*,#5839,.F.);
#7537=ORIENTED_EDGE('',*,*,#5840,.F.);
#7538=ORIENTED_EDGE('',*,*,#5841,.T.);
#7539=ORIENTED_EDGE('',*,*,#5842,.F.);
#7540=ORIENTED_EDGE('',*,*,#5843,.T.);
#7541=ORIENTED_EDGE('',*,*,#5844,.T.);
#7542=ORIENTED_EDGE('',*,*,#5845,.F.);
#7543=ORIENTED_EDGE('',*,*,#5846,.F.);
#7544=ORIENTED_EDGE('',*,*,#5847,.F.);
#7545=ORIENTED_EDGE('',*,*,#5848,.F.);
#7546=ORIENTED_EDGE('',*,*,#5849,.F.);
#7547=ORIENTED_EDGE('',*,*,#5850,.T.);
#7548=ORIENTED_EDGE('',*,*,#5851,.F.);
#7549=ORIENTED_EDGE('',*,*,#5852,.F.);
#7550=ORIENTED_EDGE('',*,*,#5853,.T.);
#7551=ORIENTED_EDGE('',*,*,#5854,.T.);
#7552=ORIENTED_EDGE('',*,*,#5855,.T.);
#7553=ORIENTED_EDGE('',*,*,#5856,.T.);
#7554=ORIENTED_EDGE('',*,*,#5857,.F.);
#7555=ORIENTED_EDGE('',*,*,#5858,.T.);
#7556=ORIENTED_EDGE('',*,*,#5859,.T.);
#7557=ORIENTED_EDGE('',*,*,#5860,.F.);
#7558=ORIENTED_EDGE('',*,*,#5861,.F.);
#7559=ORIENTED_EDGE('',*,*,#5862,.T.);
#7560=ORIENTED_EDGE('',*,*,#5863,.T.);
#7561=ORIENTED_EDGE('',*,*,#5864,.F.);
#7562=ORIENTED_EDGE('',*,*,#5865,.T.);
#7563=ORIENTED_EDGE('',*,*,#5866,.F.);
#7564=ORIENTED_EDGE('',*,*,#5867,.F.);
#7565=ORIENTED_EDGE('',*,*,#5865,.F.);
#7566=ORIENTED_EDGE('',*,*,#5868,.F.);
#7567=ORIENTED_EDGE('',*,*,#5869,.F.);
#7568=ORIENTED_EDGE('',*,*,#5870,.T.);
#7569=ORIENTED_EDGE('',*,*,#5871,.F.);
#7570=ORIENTED_EDGE('',*,*,#5870,.F.);
#7571=ORIENTED_EDGE('',*,*,#5872,.F.);
#7572=ORIENTED_EDGE('',*,*,#5873,.T.);
#7573=ORIENTED_EDGE('',*,*,#5874,.T.);
#7574=ORIENTED_EDGE('',*,*,#5873,.F.);
#7575=ORIENTED_EDGE('',*,*,#5875,.F.);
#7576=ORIENTED_EDGE('',*,*,#5876,.T.);
#7577=ORIENTED_EDGE('',*,*,#5872,.T.);
#7578=ORIENTED_EDGE('',*,*,#5876,.F.);
#7579=ORIENTED_EDGE('',*,*,#5877,.F.);
#7580=ORIENTED_EDGE('',*,*,#5878,.T.);
#7581=ORIENTED_EDGE('',*,*,#5879,.T.);
#7582=ORIENTED_EDGE('',*,*,#5878,.F.);
#7583=ORIENTED_EDGE('',*,*,#5880,.F.);
#7584=ORIENTED_EDGE('',*,*,#5881,.T.);
#7585=ORIENTED_EDGE('',*,*,#5877,.T.);
#7586=ORIENTED_EDGE('',*,*,#5881,.F.);
#7587=ORIENTED_EDGE('',*,*,#5882,.F.);
#7588=ORIENTED_EDGE('',*,*,#5883,.T.);
#7589=ORIENTED_EDGE('',*,*,#5884,.T.);
#7590=ORIENTED_EDGE('',*,*,#5883,.F.);
#7591=ORIENTED_EDGE('',*,*,#5885,.F.);
#7592=ORIENTED_EDGE('',*,*,#5886,.T.);
#7593=ORIENTED_EDGE('',*,*,#5882,.T.);
#7594=ORIENTED_EDGE('',*,*,#5886,.F.);
#7595=ORIENTED_EDGE('',*,*,#5887,.F.);
#7596=ORIENTED_EDGE('',*,*,#5888,.T.);
#7597=ORIENTED_EDGE('',*,*,#5889,.T.);
#7598=ORIENTED_EDGE('',*,*,#5888,.F.);
#7599=ORIENTED_EDGE('',*,*,#5890,.F.);
#7600=ORIENTED_EDGE('',*,*,#5891,.T.);
#7601=ORIENTED_EDGE('',*,*,#5887,.T.);
#7602=ORIENTED_EDGE('',*,*,#5891,.F.);
#7603=ORIENTED_EDGE('',*,*,#5892,.F.);
#7604=ORIENTED_EDGE('',*,*,#5893,.T.);
#7605=ORIENTED_EDGE('',*,*,#5894,.T.);
#7606=ORIENTED_EDGE('',*,*,#5893,.F.);
#7607=ORIENTED_EDGE('',*,*,#5895,.F.);
#7608=ORIENTED_EDGE('',*,*,#5896,.T.);
#7609=ORIENTED_EDGE('',*,*,#5892,.T.);
#7610=ORIENTED_EDGE('',*,*,#5896,.F.);
#7611=ORIENTED_EDGE('',*,*,#5897,.F.);
#7612=ORIENTED_EDGE('',*,*,#5898,.T.);
#7613=ORIENTED_EDGE('',*,*,#5899,.T.);
#7614=ORIENTED_EDGE('',*,*,#5898,.F.);
#7615=ORIENTED_EDGE('',*,*,#5900,.F.);
#7616=ORIENTED_EDGE('',*,*,#5901,.T.);
#7617=ORIENTED_EDGE('',*,*,#5897,.T.);
#7618=ORIENTED_EDGE('',*,*,#5901,.F.);
#7619=ORIENTED_EDGE('',*,*,#5868,.T.);
#7620=ORIENTED_EDGE('',*,*,#5869,.T.);
#7621=ORIENTED_EDGE('',*,*,#5902,.T.);
#7622=ORIENTED_EDGE('',*,*,#5866,.T.);
#7623=ORIENTED_EDGE('',*,*,#5867,.T.);
#7624=ORIENTED_EDGE('',*,*,#5902,.F.);
#7625=ORIENTED_EDGE('',*,*,#5903,.F.);
#7626=ORIENTED_EDGE('',*,*,#5904,.T.);
#7627=ORIENTED_EDGE('',*,*,#5905,.F.);
#7628=ORIENTED_EDGE('',*,*,#5904,.F.);
#7629=ORIENTED_EDGE('',*,*,#5906,.F.);
#7630=ORIENTED_EDGE('',*,*,#5907,.F.);
#7631=ORIENTED_EDGE('',*,*,#5908,.T.);
#7632=ORIENTED_EDGE('',*,*,#5909,.F.);
#7633=ORIENTED_EDGE('',*,*,#5908,.F.);
#7634=ORIENTED_EDGE('',*,*,#5906,.T.);
#7635=ORIENTED_EDGE('',*,*,#5907,.T.);
#7636=ORIENTED_EDGE('',*,*,#5910,.T.);
#7637=ORIENTED_EDGE('',*,*,#5903,.T.);
#7638=ORIENTED_EDGE('',*,*,#5910,.F.);
#7639=ORIENTED_EDGE('',*,*,#5911,.F.);
#7640=ORIENTED_EDGE('',*,*,#5912,.T.);
#7641=ORIENTED_EDGE('',*,*,#5913,.T.);
#7642=ORIENTED_EDGE('',*,*,#5912,.F.);
#7643=ORIENTED_EDGE('',*,*,#5914,.F.);
#7644=ORIENTED_EDGE('',*,*,#5915,.T.);
#7645=ORIENTED_EDGE('',*,*,#5916,.T.);
#7646=ORIENTED_EDGE('',*,*,#5915,.F.);
#7647=ORIENTED_EDGE('',*,*,#5917,.T.);
#7648=ORIENTED_EDGE('',*,*,#5918,.T.);
#7649=ORIENTED_EDGE('',*,*,#5919,.T.);
#7650=ORIENTED_EDGE('',*,*,#5918,.F.);
#7651=ORIENTED_EDGE('',*,*,#5920,.T.);
#7652=ORIENTED_EDGE('',*,*,#5921,.T.);
#7653=ORIENTED_EDGE('',*,*,#5922,.T.);
#7654=ORIENTED_EDGE('',*,*,#5921,.F.);
#7655=ORIENTED_EDGE('',*,*,#5923,.T.);
#7656=ORIENTED_EDGE('',*,*,#5924,.T.);
#7657=ORIENTED_EDGE('',*,*,#5925,.F.);
#7658=ORIENTED_EDGE('',*,*,#5926,.T.);
#7659=ORIENTED_EDGE('',*,*,#5832,.T.);
#7660=ORIENTED_EDGE('',*,*,#5927,.F.);
#7661=ORIENTED_EDGE('',*,*,#5928,.F.);
#7662=ORIENTED_EDGE('',*,*,#5926,.F.);
#7663=ORIENTED_EDGE('',*,*,#5929,.F.);
#7664=ORIENTED_EDGE('',*,*,#5930,.F.);
#7665=ORIENTED_EDGE('',*,*,#5931,.F.);
#7666=ORIENTED_EDGE('',*,*,#5932,.F.);
#7667=ORIENTED_EDGE('',*,*,#5933,.T.);
#7668=ORIENTED_EDGE('',*,*,#5932,.T.);
#7669=ORIENTED_EDGE('',*,*,#5934,.T.);
#7670=ORIENTED_EDGE('',*,*,#5935,.F.);
#7671=ORIENTED_EDGE('',*,*,#5936,.F.);
#7672=ORIENTED_EDGE('',*,*,#5937,.F.);
#7673=ORIENTED_EDGE('',*,*,#5938,.T.);
#7674=ORIENTED_EDGE('',*,*,#5939,.T.);
#7675=ORIENTED_EDGE('',*,*,#5940,.F.);
#7676=ORIENTED_EDGE('',*,*,#5835,.T.);
#7677=ORIENTED_EDGE('',*,*,#5836,.T.);
#7678=ORIENTED_EDGE('',*,*,#5941,.T.);
#7679=ORIENTED_EDGE('',*,*,#5942,.F.);
#7680=ORIENTED_EDGE('',*,*,#5943,.T.);
#7681=ORIENTED_EDGE('',*,*,#5944,.F.);
#7682=ORIENTED_EDGE('',*,*,#5943,.F.);
#7683=ORIENTED_EDGE('',*,*,#5945,.T.);
#7684=ORIENTED_EDGE('',*,*,#5946,.T.);
#7685=ORIENTED_EDGE('',*,*,#5947,.T.);
#7686=ORIENTED_EDGE('',*,*,#5937,.T.);
#7687=ORIENTED_EDGE('',*,*,#5948,.T.);
#7688=ORIENTED_EDGE('',*,*,#5949,.T.);
#7689=ORIENTED_EDGE('',*,*,#5950,.T.);
#7690=ORIENTED_EDGE('',*,*,#5941,.F.);
#7691=ORIENTED_EDGE('',*,*,#5951,.T.);
#7692=ORIENTED_EDGE('',*,*,#5952,.T.);
#7693=ORIENTED_EDGE('',*,*,#5953,.T.);
#7694=ORIENTED_EDGE('',*,*,#5954,.T.);
#7695=ORIENTED_EDGE('',*,*,#5955,.T.);
#7696=ORIENTED_EDGE('',*,*,#5851,.T.);
#7697=ORIENTED_EDGE('',*,*,#5956,.F.);
#7698=ORIENTED_EDGE('',*,*,#5957,.T.);
#7699=ORIENTED_EDGE('',*,*,#5958,.T.);
#7700=ORIENTED_EDGE('',*,*,#5959,.T.);
#7701=ORIENTED_EDGE('',*,*,#5960,.T.);
#7702=ORIENTED_EDGE('',*,*,#5961,.T.);
#7703=ORIENTED_EDGE('',*,*,#5962,.F.);
#7704=ORIENTED_EDGE('',*,*,#5847,.T.);
#7705=ORIENTED_EDGE('',*,*,#5963,.T.);
#7706=ORIENTED_EDGE('',*,*,#5964,.T.);
#7707=ORIENTED_EDGE('',*,*,#5965,.T.);
#7708=ORIENTED_EDGE('',*,*,#5966,.T.);
#7709=ORIENTED_EDGE('',*,*,#5967,.T.);
#7710=ORIENTED_EDGE('',*,*,#5842,.T.);
#7711=ORIENTED_EDGE('',*,*,#5968,.T.);
#7712=ORIENTED_EDGE('',*,*,#5969,.T.);
#7713=ORIENTED_EDGE('',*,*,#5970,.T.);
#7714=ORIENTED_EDGE('',*,*,#5971,.T.);
#7715=ORIENTED_EDGE('',*,*,#5972,.T.);
#7716=ORIENTED_EDGE('',*,*,#5973,.T.);
#7717=ORIENTED_EDGE('',*,*,#5974,.T.);
#7718=ORIENTED_EDGE('',*,*,#5975,.T.);
#7719=ORIENTED_EDGE('',*,*,#5976,.T.);
#7720=ORIENTED_EDGE('',*,*,#5977,.T.);
#7721=ORIENTED_EDGE('',*,*,#5978,.T.);
#7722=ORIENTED_EDGE('',*,*,#5979,.T.);
#7723=ORIENTED_EDGE('',*,*,#5980,.F.);
#7724=ORIENTED_EDGE('',*,*,#5981,.T.);
#7725=ORIENTED_EDGE('',*,*,#5982,.T.);
#7726=ORIENTED_EDGE('',*,*,#5983,.T.);
#7727=ORIENTED_EDGE('',*,*,#5984,.T.);
#7728=ORIENTED_EDGE('',*,*,#5985,.T.);
#7729=ORIENTED_EDGE('',*,*,#5986,.F.);
#7730=ORIENTED_EDGE('',*,*,#5987,.T.);
#7731=ORIENTED_EDGE('',*,*,#5988,.T.);
#7732=ORIENTED_EDGE('',*,*,#5989,.T.);
#7733=ORIENTED_EDGE('',*,*,#5990,.T.);
#7734=ORIENTED_EDGE('',*,*,#5991,.T.);
#7735=ORIENTED_EDGE('',*,*,#5992,.T.);
#7736=ORIENTED_EDGE('',*,*,#5993,.T.);
#7737=ORIENTED_EDGE('',*,*,#5913,.F.);
#7738=ORIENTED_EDGE('',*,*,#5916,.F.);
#7739=ORIENTED_EDGE('',*,*,#5994,.T.);
#7740=ORIENTED_EDGE('',*,*,#5995,.T.);
#7741=ORIENTED_EDGE('',*,*,#5996,.T.);
#7742=ORIENTED_EDGE('',*,*,#5997,.T.);
#7743=ORIENTED_EDGE('',*,*,#5998,.T.);
#7744=ORIENTED_EDGE('',*,*,#5999,.T.);
#7745=ORIENTED_EDGE('',*,*,#6000,.F.);
#7746=ORIENTED_EDGE('',*,*,#6001,.T.);
#7747=ORIENTED_EDGE('',*,*,#6002,.F.);
#7748=ORIENTED_EDGE('',*,*,#6003,.T.);
#7749=ORIENTED_EDGE('',*,*,#6004,.T.);
#7750=ORIENTED_EDGE('',*,*,#6005,.T.);
#7751=ORIENTED_EDGE('',*,*,#6006,.F.);
#7752=ORIENTED_EDGE('',*,*,#6007,.T.);
#7753=ORIENTED_EDGE('',*,*,#6008,.F.);
#7754=ORIENTED_EDGE('',*,*,#6009,.T.);
#7755=ORIENTED_EDGE('',*,*,#6010,.T.);
#7756=ORIENTED_EDGE('',*,*,#6011,.T.);
#7757=ORIENTED_EDGE('',*,*,#5911,.T.);
#7758=ORIENTED_EDGE('',*,*,#5914,.T.);
#7759=ORIENTED_EDGE('',*,*,#6012,.T.);
#7760=ORIENTED_EDGE('',*,*,#5845,.T.);
#7761=ORIENTED_EDGE('',*,*,#6013,.T.);
#7762=ORIENTED_EDGE('',*,*,#6014,.T.);
#7763=ORIENTED_EDGE('',*,*,#6015,.T.);
#7764=ORIENTED_EDGE('',*,*,#6016,.T.);
#7765=ORIENTED_EDGE('',*,*,#6017,.T.);
#7766=ORIENTED_EDGE('',*,*,#5849,.T.);
#7767=ORIENTED_EDGE('',*,*,#6018,.T.);
#7768=ORIENTED_EDGE('',*,*,#6019,.F.);
#7769=ORIENTED_EDGE('',*,*,#6020,.T.);
#7770=ORIENTED_EDGE('',*,*,#6021,.F.);
#7771=ORIENTED_EDGE('',*,*,#6022,.T.);
#7772=ORIENTED_EDGE('',*,*,#5840,.T.);
#7773=ORIENTED_EDGE('',*,*,#6023,.T.);
#7774=ORIENTED_EDGE('',*,*,#6024,.F.);
#7775=ORIENTED_EDGE('',*,*,#6025,.T.);
#7776=ORIENTED_EDGE('',*,*,#6026,.F.);
#7777=ORIENTED_EDGE('',*,*,#5917,.F.);
#7778=ORIENTED_EDGE('',*,*,#5920,.F.);
#7779=ORIENTED_EDGE('',*,*,#5838,.T.);
#7780=ORIENTED_EDGE('',*,*,#5905,.T.);
#7781=ORIENTED_EDGE('',*,*,#6027,.T.);
#7782=ORIENTED_EDGE('',*,*,#5940,.T.);
#7783=ORIENTED_EDGE('',*,*,#6028,.T.);
#7784=ORIENTED_EDGE('',*,*,#6029,.T.);
#7785=ORIENTED_EDGE('',*,*,#6030,.T.);
#7786=ORIENTED_EDGE('',*,*,#6031,.T.);
#7787=ORIENTED_EDGE('',*,*,#6032,.T.);
#7788=ORIENTED_EDGE('',*,*,#6033,.T.);
#7789=ORIENTED_EDGE('',*,*,#6034,.T.);
#7790=ORIENTED_EDGE('',*,*,#5942,.T.);
#7791=ORIENTED_EDGE('',*,*,#6035,.T.);
#7792=ORIENTED_EDGE('',*,*,#6036,.T.);
#7793=ORIENTED_EDGE('',*,*,#6037,.F.);
#7794=ORIENTED_EDGE('',*,*,#6038,.T.);
#7795=ORIENTED_EDGE('',*,*,#6039,.T.);
#7796=ORIENTED_EDGE('',*,*,#6040,.T.);
#7797=ORIENTED_EDGE('',*,*,#6041,.T.);
#7798=ORIENTED_EDGE('',*,*,#6042,.T.);
#7799=ORIENTED_EDGE('',*,*,#6043,.T.);
#7800=ORIENTED_EDGE('',*,*,#6044,.T.);
#7801=ORIENTED_EDGE('',*,*,#6045,.T.);
#7802=ORIENTED_EDGE('',*,*,#6046,.T.);
#7803=ORIENTED_EDGE('',*,*,#6047,.T.);
#7804=ORIENTED_EDGE('',*,*,#6048,.T.);
#7805=ORIENTED_EDGE('',*,*,#6049,.T.);
#7806=ORIENTED_EDGE('',*,*,#6050,.T.);
#7807=ORIENTED_EDGE('',*,*,#6051,.T.);
#7808=ORIENTED_EDGE('',*,*,#6052,.T.);
#7809=ORIENTED_EDGE('',*,*,#6053,.F.);
#7810=ORIENTED_EDGE('',*,*,#6054,.F.);
#7811=ORIENTED_EDGE('',*,*,#6055,.F.);
#7812=ORIENTED_EDGE('',*,*,#6056,.F.);
#7813=ORIENTED_EDGE('',*,*,#6057,.F.);
#7814=ORIENTED_EDGE('',*,*,#6058,.F.);
#7815=ORIENTED_EDGE('',*,*,#6059,.F.);
#7816=ORIENTED_EDGE('',*,*,#6060,.F.);
#7817=ORIENTED_EDGE('',*,*,#6037,.T.);
#7818=ORIENTED_EDGE('',*,*,#6061,.T.);
#7819=ORIENTED_EDGE('',*,*,#6062,.T.);
#7820=ORIENTED_EDGE('',*,*,#6051,.F.);
#7821=ORIENTED_EDGE('',*,*,#6063,.T.);
#7822=ORIENTED_EDGE('',*,*,#6064,.T.);
#7823=ORIENTED_EDGE('',*,*,#6065,.T.);
#7824=ORIENTED_EDGE('',*,*,#6066,.T.);
#7825=ORIENTED_EDGE('',*,*,#6067,.T.);
#7826=ORIENTED_EDGE('',*,*,#6068,.T.);
#7827=ORIENTED_EDGE('',*,*,#6049,.F.);
#7828=ORIENTED_EDGE('',*,*,#6069,.T.);
#7829=ORIENTED_EDGE('',*,*,#6070,.T.);
#7830=ORIENTED_EDGE('',*,*,#6071,.T.);
#7831=ORIENTED_EDGE('',*,*,#6045,.F.);
#7832=ORIENTED_EDGE('',*,*,#6072,.T.);
#7833=ORIENTED_EDGE('',*,*,#6047,.F.);
#7834=ORIENTED_EDGE('',*,*,#6073,.T.);
#7835=ORIENTED_EDGE('',*,*,#6074,.T.);
#7836=ORIENTED_EDGE('',*,*,#6075,.T.);
#7837=ORIENTED_EDGE('',*,*,#6067,.F.);
#7838=ORIENTED_EDGE('',*,*,#6076,.T.);
#7839=ORIENTED_EDGE('',*,*,#6033,.F.);
#7840=ORIENTED_EDGE('',*,*,#6077,.T.);
#7841=ORIENTED_EDGE('',*,*,#6078,.T.);
#7842=ORIENTED_EDGE('',*,*,#6079,.T.);
#7843=ORIENTED_EDGE('',*,*,#6080,.T.);
#7844=ORIENTED_EDGE('',*,*,#6029,.F.);
#7845=ORIENTED_EDGE('',*,*,#6081,.T.);
#7846=ORIENTED_EDGE('',*,*,#6082,.T.);
#7847=ORIENTED_EDGE('',*,*,#6083,.T.);
#7848=ORIENTED_EDGE('',*,*,#6074,.F.);
#7849=ORIENTED_EDGE('',*,*,#6084,.T.);
#7850=ORIENTED_EDGE('',*,*,#6044,.F.);
#7851=ORIENTED_EDGE('',*,*,#6085,.T.);
#7852=ORIENTED_EDGE('',*,*,#6069,.F.);
#7853=ORIENTED_EDGE('',*,*,#6086,.T.);
#7854=ORIENTED_EDGE('',*,*,#6087,.T.);
#7855=ORIENTED_EDGE('',*,*,#6046,.F.);
#7856=ORIENTED_EDGE('',*,*,#6071,.F.);
#7857=ORIENTED_EDGE('',*,*,#6088,.F.);
#7858=ORIENTED_EDGE('',*,*,#6073,.F.);
#7859=ORIENTED_EDGE('',*,*,#6088,.T.);
#7860=ORIENTED_EDGE('',*,*,#6070,.F.);
#7861=ORIENTED_EDGE('',*,*,#6089,.F.);
#7862=ORIENTED_EDGE('',*,*,#6084,.F.);
#7863=ORIENTED_EDGE('',*,*,#6089,.T.);
#7864=ORIENTED_EDGE('',*,*,#6085,.F.);
#7865=ORIENTED_EDGE('',*,*,#6090,.F.);
#7866=ORIENTED_EDGE('',*,*,#6079,.F.);
#7867=ORIENTED_EDGE('',*,*,#6090,.T.);
#7868=ORIENTED_EDGE('',*,*,#6043,.F.);
#7869=ORIENTED_EDGE('',*,*,#6091,.F.);
#7870=ORIENTED_EDGE('',*,*,#6080,.F.);
#7871=ORIENTED_EDGE('',*,*,#6042,.F.);
#7872=ORIENTED_EDGE('',*,*,#6092,.T.);
#7873=ORIENTED_EDGE('',*,*,#6027,.F.);
#7874=ORIENTED_EDGE('',*,*,#6091,.T.);
#7875=ORIENTED_EDGE('',*,*,#6048,.F.);
#7876=ORIENTED_EDGE('',*,*,#6075,.F.);
#7877=ORIENTED_EDGE('',*,*,#6093,.F.);
#7878=ORIENTED_EDGE('',*,*,#6065,.F.);
#7879=ORIENTED_EDGE('',*,*,#6093,.T.);
#7880=ORIENTED_EDGE('',*,*,#6083,.F.);
#7881=ORIENTED_EDGE('',*,*,#6094,.F.);
#7882=ORIENTED_EDGE('',*,*,#6066,.F.);
#7883=ORIENTED_EDGE('',*,*,#6094,.T.);
#7884=ORIENTED_EDGE('',*,*,#6082,.F.);
#7885=ORIENTED_EDGE('',*,*,#6095,.F.);
#7886=ORIENTED_EDGE('',*,*,#6076,.F.);
#7887=ORIENTED_EDGE('',*,*,#6095,.T.);
#7888=ORIENTED_EDGE('',*,*,#6081,.F.);
#7889=ORIENTED_EDGE('',*,*,#6096,.F.);
#7890=ORIENTED_EDGE('',*,*,#6034,.F.);
#7891=ORIENTED_EDGE('',*,*,#6028,.F.);
#7892=ORIENTED_EDGE('',*,*,#6097,.T.);
#7893=ORIENTED_EDGE('',*,*,#6030,.F.);
#7894=ORIENTED_EDGE('',*,*,#6096,.T.);
#7895=ORIENTED_EDGE('',*,*,#6052,.F.);
#7896=ORIENTED_EDGE('',*,*,#6062,.F.);
#7897=ORIENTED_EDGE('',*,*,#6098,.F.);
#7898=ORIENTED_EDGE('',*,*,#6072,.F.);
#7899=ORIENTED_EDGE('',*,*,#6098,.T.);
#7900=ORIENTED_EDGE('',*,*,#6061,.F.);
#7901=ORIENTED_EDGE('',*,*,#6099,.F.);
#7902=ORIENTED_EDGE('',*,*,#6086,.F.);
#7903=ORIENTED_EDGE('',*,*,#6099,.T.);
#7904=ORIENTED_EDGE('',*,*,#6036,.F.);
#7905=ORIENTED_EDGE('',*,*,#6100,.F.);
#7906=ORIENTED_EDGE('',*,*,#6087,.F.);
#7907=ORIENTED_EDGE('',*,*,#6035,.F.);
#7908=ORIENTED_EDGE('',*,*,#6101,.T.);
#7909=ORIENTED_EDGE('',*,*,#6040,.F.);
#7910=ORIENTED_EDGE('',*,*,#6100,.T.);
#7911=ORIENTED_EDGE('',*,*,#6050,.F.);
#7912=ORIENTED_EDGE('',*,*,#6068,.F.);
#7913=ORIENTED_EDGE('',*,*,#6102,.F.);
#7914=ORIENTED_EDGE('',*,*,#6063,.F.);
#7915=ORIENTED_EDGE('',*,*,#6102,.T.);
#7916=ORIENTED_EDGE('',*,*,#6078,.F.);
#7917=ORIENTED_EDGE('',*,*,#6103,.F.);
#7918=ORIENTED_EDGE('',*,*,#6064,.F.);
#7919=ORIENTED_EDGE('',*,*,#6103,.T.);
#7920=ORIENTED_EDGE('',*,*,#6077,.F.);
#7921=ORIENTED_EDGE('',*,*,#6104,.F.);
#7922=ORIENTED_EDGE('',*,*,#6038,.F.);
#7923=ORIENTED_EDGE('',*,*,#6032,.F.);
#7924=ORIENTED_EDGE('',*,*,#6105,.T.);
#7925=ORIENTED_EDGE('',*,*,#6039,.F.);
#7926=ORIENTED_EDGE('',*,*,#6104,.T.);
#7927=ORIENTED_EDGE('',*,*,#5945,.F.);
#7928=ORIENTED_EDGE('',*,*,#6105,.F.);
#7929=ORIENTED_EDGE('',*,*,#6106,.F.);
#7930=ORIENTED_EDGE('',*,*,#6106,.T.);
#7931=ORIENTED_EDGE('',*,*,#6031,.F.);
#7932=ORIENTED_EDGE('',*,*,#6107,.F.);
#7933=ORIENTED_EDGE('',*,*,#5946,.F.);
#7934=ORIENTED_EDGE('',*,*,#6107,.T.);
#7935=ORIENTED_EDGE('',*,*,#6097,.F.);
#7936=ORIENTED_EDGE('',*,*,#5939,.F.);
#7937=ORIENTED_EDGE('',*,*,#5938,.F.);
#7938=ORIENTED_EDGE('',*,*,#5947,.F.);
#7939=ORIENTED_EDGE('',*,*,#5936,.T.);
#7940=ORIENTED_EDGE('',*,*,#5935,.T.);
#7941=ORIENTED_EDGE('',*,*,#6092,.F.);
#7942=ORIENTED_EDGE('',*,*,#6108,.F.);
#7943=ORIENTED_EDGE('',*,*,#5948,.F.);
#7944=ORIENTED_EDGE('',*,*,#6108,.T.);
#7945=ORIENTED_EDGE('',*,*,#6041,.F.);
#7946=ORIENTED_EDGE('',*,*,#6109,.F.);
#7947=ORIENTED_EDGE('',*,*,#5949,.F.);
#7948=ORIENTED_EDGE('',*,*,#6109,.T.);
#7949=ORIENTED_EDGE('',*,*,#6101,.F.);
#7950=ORIENTED_EDGE('',*,*,#5950,.F.);
#7951=ORIENTED_EDGE('',*,*,#5927,.T.);
#7952=ORIENTED_EDGE('',*,*,#5834,.T.);
#7953=ORIENTED_EDGE('',*,*,#6110,.F.);
#7954=ORIENTED_EDGE('',*,*,#5909,.T.);
#7955=ORIENTED_EDGE('',*,*,#6111,.F.);
#7956=ORIENTED_EDGE('',*,*,#6112,.F.);
#7957=ORIENTED_EDGE('',*,*,#6113,.F.);
#7958=ORIENTED_EDGE('',*,*,#5924,.F.);
#7959=ORIENTED_EDGE('',*,*,#6114,.F.);
#7960=ORIENTED_EDGE('',*,*,#6115,.F.);
#7961=ORIENTED_EDGE('',*,*,#6116,.F.);
#7962=ORIENTED_EDGE('',*,*,#6117,.F.);
#7963=ORIENTED_EDGE('',*,*,#6118,.F.);
#7964=ORIENTED_EDGE('',*,*,#5934,.F.);
#7965=ORIENTED_EDGE('',*,*,#6119,.F.);
#7966=ORIENTED_EDGE('',*,*,#6120,.F.);
#7967=ORIENTED_EDGE('',*,*,#6121,.T.);
#7968=ORIENTED_EDGE('',*,*,#6122,.F.);
#7969=ORIENTED_EDGE('',*,*,#6123,.F.);
#7970=ORIENTED_EDGE('',*,*,#6124,.F.);
#7971=ORIENTED_EDGE('',*,*,#6125,.F.);
#7972=ORIENTED_EDGE('',*,*,#6126,.F.);
#7973=ORIENTED_EDGE('',*,*,#6127,.F.);
#7974=ORIENTED_EDGE('',*,*,#6128,.F.);
#7975=ORIENTED_EDGE('',*,*,#6121,.F.);
#7976=ORIENTED_EDGE('',*,*,#6129,.F.);
#7977=ORIENTED_EDGE('',*,*,#6130,.F.);
#7978=ORIENTED_EDGE('',*,*,#6055,.T.);
#7979=ORIENTED_EDGE('',*,*,#6131,.F.);
#7980=ORIENTED_EDGE('',*,*,#6132,.F.);
#7981=ORIENTED_EDGE('',*,*,#6133,.F.);
#7982=ORIENTED_EDGE('',*,*,#6057,.T.);
#7983=ORIENTED_EDGE('',*,*,#6134,.F.);
#7984=ORIENTED_EDGE('',*,*,#6135,.F.);
#7985=ORIENTED_EDGE('',*,*,#6136,.F.);
#7986=ORIENTED_EDGE('',*,*,#6137,.F.);
#7987=ORIENTED_EDGE('',*,*,#6138,.F.);
#7988=ORIENTED_EDGE('',*,*,#6053,.T.);
#7989=ORIENTED_EDGE('',*,*,#6139,.F.);
#7990=ORIENTED_EDGE('',*,*,#6140,.F.);
#7991=ORIENTED_EDGE('',*,*,#6059,.T.);
#7992=ORIENTED_EDGE('',*,*,#6141,.F.);
#7993=ORIENTED_EDGE('',*,*,#6142,.F.);
#7994=ORIENTED_EDGE('',*,*,#6143,.F.);
#7995=ORIENTED_EDGE('',*,*,#6135,.T.);
#7996=ORIENTED_EDGE('',*,*,#6144,.F.);
#7997=ORIENTED_EDGE('',*,*,#6145,.F.);
#7998=ORIENTED_EDGE('',*,*,#6116,.T.);
#7999=ORIENTED_EDGE('',*,*,#6146,.F.);
#8000=ORIENTED_EDGE('',*,*,#6147,.F.);
#8001=ORIENTED_EDGE('',*,*,#6148,.F.);
#8002=ORIENTED_EDGE('',*,*,#6142,.T.);
#8003=ORIENTED_EDGE('',*,*,#6149,.F.);
#8004=ORIENTED_EDGE('',*,*,#6150,.F.);
#8005=ORIENTED_EDGE('',*,*,#6151,.F.);
#8006=ORIENTED_EDGE('',*,*,#6112,.T.);
#8007=ORIENTED_EDGE('',*,*,#6152,.F.);
#8008=ORIENTED_EDGE('',*,*,#6125,.T.);
#8009=ORIENTED_EDGE('',*,*,#6153,.F.);
#8010=ORIENTED_EDGE('',*,*,#6154,.F.);
#8011=ORIENTED_EDGE('',*,*,#6137,.T.);
#8012=ORIENTED_EDGE('',*,*,#6155,.F.);
#8013=ORIENTED_EDGE('',*,*,#6060,.T.);
#8014=ORIENTED_EDGE('',*,*,#6143,.T.);
#8015=ORIENTED_EDGE('',*,*,#6156,.T.);
#8016=ORIENTED_EDGE('',*,*,#6139,.T.);
#8017=ORIENTED_EDGE('',*,*,#6156,.F.);
#8018=ORIENTED_EDGE('',*,*,#6148,.T.);
#8019=ORIENTED_EDGE('',*,*,#6157,.T.);
#8020=ORIENTED_EDGE('',*,*,#6140,.T.);
#8021=ORIENTED_EDGE('',*,*,#6157,.F.);
#8022=ORIENTED_EDGE('',*,*,#6147,.T.);
#8023=ORIENTED_EDGE('',*,*,#6158,.T.);
#8024=ORIENTED_EDGE('',*,*,#6155,.T.);
#8025=ORIENTED_EDGE('',*,*,#6158,.F.);
#8026=ORIENTED_EDGE('',*,*,#6152,.T.);
#8027=ORIENTED_EDGE('',*,*,#6159,.T.);
#8028=ORIENTED_EDGE('',*,*,#6126,.T.);
#8029=ORIENTED_EDGE('',*,*,#6127,.T.);
#8030=ORIENTED_EDGE('',*,*,#6159,.F.);
#8031=ORIENTED_EDGE('',*,*,#6111,.T.);
#8032=ORIENTED_EDGE('',*,*,#6160,.F.);
#8033=ORIENTED_EDGE('',*,*,#6058,.T.);
#8034=ORIENTED_EDGE('',*,*,#6133,.T.);
#8035=ORIENTED_EDGE('',*,*,#6161,.T.);
#8036=ORIENTED_EDGE('',*,*,#6141,.T.);
#8037=ORIENTED_EDGE('',*,*,#6161,.F.);
#8038=ORIENTED_EDGE('',*,*,#6136,.T.);
#8039=ORIENTED_EDGE('',*,*,#6162,.T.);
#8040=ORIENTED_EDGE('',*,*,#6149,.T.);
#8041=ORIENTED_EDGE('',*,*,#6162,.F.);
#8042=ORIENTED_EDGE('',*,*,#6146,.T.);
#8043=ORIENTED_EDGE('',*,*,#6163,.T.);
#8044=ORIENTED_EDGE('',*,*,#6150,.T.);
#8045=ORIENTED_EDGE('',*,*,#6163,.F.);
#8046=ORIENTED_EDGE('',*,*,#6115,.T.);
#8047=ORIENTED_EDGE('',*,*,#6164,.T.);
#8048=ORIENTED_EDGE('',*,*,#6151,.T.);
#8049=ORIENTED_EDGE('',*,*,#6113,.T.);
#8050=ORIENTED_EDGE('',*,*,#6164,.F.);
#8051=ORIENTED_EDGE('',*,*,#6114,.T.);
#8052=ORIENTED_EDGE('',*,*,#6165,.F.);
#8053=ORIENTED_EDGE('',*,*,#6054,.T.);
#8054=ORIENTED_EDGE('',*,*,#6138,.T.);
#8055=ORIENTED_EDGE('',*,*,#6166,.T.);
#8056=ORIENTED_EDGE('',*,*,#6131,.T.);
#8057=ORIENTED_EDGE('',*,*,#6166,.F.);
#8058=ORIENTED_EDGE('',*,*,#6154,.T.);
#8059=ORIENTED_EDGE('',*,*,#6167,.T.);
#8060=ORIENTED_EDGE('',*,*,#6132,.T.);
#8061=ORIENTED_EDGE('',*,*,#6167,.F.);
#8062=ORIENTED_EDGE('',*,*,#6153,.T.);
#8063=ORIENTED_EDGE('',*,*,#6168,.T.);
#8064=ORIENTED_EDGE('',*,*,#6122,.T.);
#8065=ORIENTED_EDGE('',*,*,#6123,.T.);
#8066=ORIENTED_EDGE('',*,*,#6168,.F.);
#8067=ORIENTED_EDGE('',*,*,#6124,.T.);
#8068=ORIENTED_EDGE('',*,*,#6169,.F.);
#8069=ORIENTED_EDGE('',*,*,#6056,.T.);
#8070=ORIENTED_EDGE('',*,*,#6130,.T.);
#8071=ORIENTED_EDGE('',*,*,#6170,.T.);
#8072=ORIENTED_EDGE('',*,*,#6134,.T.);
#8073=ORIENTED_EDGE('',*,*,#6170,.F.);
#8074=ORIENTED_EDGE('',*,*,#6129,.T.);
#8075=ORIENTED_EDGE('',*,*,#6171,.T.);
#8076=ORIENTED_EDGE('',*,*,#6144,.T.);
#8077=ORIENTED_EDGE('',*,*,#6171,.F.);
#8078=ORIENTED_EDGE('',*,*,#6120,.T.);
#8079=ORIENTED_EDGE('',*,*,#6172,.T.);
#8080=ORIENTED_EDGE('',*,*,#6145,.T.);
#8081=ORIENTED_EDGE('',*,*,#6117,.T.);
#8082=ORIENTED_EDGE('',*,*,#6172,.F.);
#8083=ORIENTED_EDGE('',*,*,#6119,.T.);
#8084=ORIENTED_EDGE('',*,*,#6173,.F.);
#8085=ORIENTED_EDGE('',*,*,#5931,.T.);
#8086=ORIENTED_EDGE('',*,*,#6174,.T.);
#8087=ORIENTED_EDGE('',*,*,#6173,.T.);
#8088=ORIENTED_EDGE('',*,*,#6174,.F.);
#8089=ORIENTED_EDGE('',*,*,#5930,.T.);
#8090=ORIENTED_EDGE('',*,*,#6175,.T.);
#8091=ORIENTED_EDGE('',*,*,#6118,.T.);
#8092=ORIENTED_EDGE('',*,*,#6175,.F.);
#8093=ORIENTED_EDGE('',*,*,#5929,.T.);
#8094=ORIENTED_EDGE('',*,*,#5925,.T.);
#8095=ORIENTED_EDGE('',*,*,#6165,.T.);
#8096=ORIENTED_EDGE('',*,*,#5923,.F.);
#8097=ORIENTED_EDGE('',*,*,#5928,.T.);
#8098=ORIENTED_EDGE('',*,*,#6176,.T.);
#8099=ORIENTED_EDGE('',*,*,#6160,.T.);
#8100=ORIENTED_EDGE('',*,*,#6176,.F.);
#8101=ORIENTED_EDGE('',*,*,#6110,.T.);
#8102=ORIENTED_EDGE('',*,*,#6177,.T.);
#8103=ORIENTED_EDGE('',*,*,#6128,.T.);
#8104=ORIENTED_EDGE('',*,*,#6177,.F.);
#8105=ORIENTED_EDGE('',*,*,#5833,.T.);
#8106=ORIENTED_EDGE('',*,*,#6169,.T.);
#8107=ORIENTED_EDGE('',*,*,#6178,.T.);
#8108=ORIENTED_EDGE('',*,*,#6179,.T.);
#8109=ORIENTED_EDGE('',*,*,#6180,.T.);
#8110=ORIENTED_EDGE('',*,*,#6181,.T.);
#8111=ORIENTED_EDGE('',*,*,#6182,.T.);
#8112=ORIENTED_EDGE('',*,*,#6183,.T.);
#8113=ORIENTED_EDGE('',*,*,#6184,.T.);
#8114=ORIENTED_EDGE('',*,*,#6185,.T.);
#8115=ORIENTED_EDGE('',*,*,#6186,.T.);
#8116=ORIENTED_EDGE('',*,*,#6187,.T.);
#8117=ORIENTED_EDGE('',*,*,#5919,.F.);
#8118=ORIENTED_EDGE('',*,*,#5922,.F.);
#8119=ORIENTED_EDGE('',*,*,#6188,.T.);
#8120=ORIENTED_EDGE('',*,*,#6189,.T.);
#8121=ORIENTED_EDGE('',*,*,#6190,.T.);
#8122=ORIENTED_EDGE('',*,*,#6191,.T.);
#8123=ORIENTED_EDGE('',*,*,#6192,.T.);
#8124=ORIENTED_EDGE('',*,*,#6193,.T.);
#8125=ORIENTED_EDGE('',*,*,#6194,.T.);
#8126=ORIENTED_EDGE('',*,*,#6195,.T.);
#8127=ORIENTED_EDGE('',*,*,#6196,.T.);
#8128=ORIENTED_EDGE('',*,*,#6197,.T.);
#8129=ORIENTED_EDGE('',*,*,#6198,.T.);
#8130=ORIENTED_EDGE('',*,*,#6199,.T.);
#8131=ORIENTED_EDGE('',*,*,#6200,.T.);
#8132=ORIENTED_EDGE('',*,*,#6201,.T.);
#8133=ORIENTED_EDGE('',*,*,#6202,.T.);
#8134=ORIENTED_EDGE('',*,*,#6203,.T.);
#8135=ORIENTED_EDGE('',*,*,#6204,.T.);
#8136=ORIENTED_EDGE('',*,*,#6205,.T.);
#8137=ORIENTED_EDGE('',*,*,#6206,.T.);
#8138=ORIENTED_EDGE('',*,*,#6207,.T.);
#8139=ORIENTED_EDGE('',*,*,#6208,.T.);
#8140=ORIENTED_EDGE('',*,*,#6209,.T.);
#8141=ORIENTED_EDGE('',*,*,#6210,.T.);
#8142=ORIENTED_EDGE('',*,*,#6211,.T.);
#8143=ORIENTED_EDGE('',*,*,#6212,.T.);
#8144=ORIENTED_EDGE('',*,*,#6213,.T.);
#8145=ORIENTED_EDGE('',*,*,#6214,.T.);
#8146=ORIENTED_EDGE('',*,*,#6215,.T.);
#8147=ORIENTED_EDGE('',*,*,#6216,.T.);
#8148=ORIENTED_EDGE('',*,*,#6217,.T.);
#8149=ORIENTED_EDGE('',*,*,#6218,.T.);
#8150=ORIENTED_EDGE('',*,*,#6219,.T.);
#8151=ORIENTED_EDGE('',*,*,#6220,.T.);
#8152=ORIENTED_EDGE('',*,*,#6221,.T.);
#8153=ORIENTED_EDGE('',*,*,#6222,.T.);
#8154=ORIENTED_EDGE('',*,*,#6223,.T.);
#8155=ORIENTED_EDGE('',*,*,#6224,.T.);
#8156=ORIENTED_EDGE('',*,*,#6225,.T.);
#8157=ORIENTED_EDGE('',*,*,#6226,.T.);
#8158=ORIENTED_EDGE('',*,*,#6227,.T.);
#8159=ORIENTED_EDGE('',*,*,#6228,.T.);
#8160=ORIENTED_EDGE('',*,*,#6229,.T.);
#8161=ORIENTED_EDGE('',*,*,#6230,.T.);
#8162=ORIENTED_EDGE('',*,*,#6231,.T.);
#8163=ORIENTED_EDGE('',*,*,#6232,.T.);
#8164=ORIENTED_EDGE('',*,*,#6233,.T.);
#8165=ORIENTED_EDGE('',*,*,#6234,.T.);
#8166=ORIENTED_EDGE('',*,*,#6235,.T.);
#8167=ORIENTED_EDGE('',*,*,#6236,.T.);
#8168=ORIENTED_EDGE('',*,*,#6237,.T.);
#8169=ORIENTED_EDGE('',*,*,#6238,.T.);
#8170=ORIENTED_EDGE('',*,*,#6239,.T.);
#8171=ORIENTED_EDGE('',*,*,#6240,.T.);
#8172=ORIENTED_EDGE('',*,*,#6241,.T.);
#8173=ORIENTED_EDGE('',*,*,#6242,.T.);
#8174=ORIENTED_EDGE('',*,*,#6243,.T.);
#8175=ORIENTED_EDGE('',*,*,#6244,.T.);
#8176=ORIENTED_EDGE('',*,*,#6245,.T.);
#8177=ORIENTED_EDGE('',*,*,#6246,.T.);
#8178=ORIENTED_EDGE('',*,*,#6247,.T.);
#8179=ORIENTED_EDGE('',*,*,#6248,.T.);
#8180=ORIENTED_EDGE('',*,*,#6249,.T.);
#8181=ORIENTED_EDGE('',*,*,#6250,.T.);
#8182=ORIENTED_EDGE('',*,*,#6251,.T.);
#8183=ORIENTED_EDGE('',*,*,#6252,.T.);
#8184=ORIENTED_EDGE('',*,*,#6253,.T.);
#8185=ORIENTED_EDGE('',*,*,#6254,.T.);
#8186=ORIENTED_EDGE('',*,*,#6255,.T.);
#8187=ORIENTED_EDGE('',*,*,#6256,.T.);
#8188=ORIENTED_EDGE('',*,*,#6257,.T.);
#8189=ORIENTED_EDGE('',*,*,#6258,.T.);
#8190=ORIENTED_EDGE('',*,*,#6259,.T.);
#8191=ORIENTED_EDGE('',*,*,#6260,.T.);
#8192=ORIENTED_EDGE('',*,*,#6261,.T.);
#8193=ORIENTED_EDGE('',*,*,#6262,.T.);
#8194=ORIENTED_EDGE('',*,*,#6263,.T.);
#8195=ORIENTED_EDGE('',*,*,#5871,.T.);
#8196=ORIENTED_EDGE('',*,*,#5944,.T.);
#8197=ORIENTED_EDGE('',*,*,#5900,.T.);
#8198=ORIENTED_EDGE('',*,*,#5895,.T.);
#8199=ORIENTED_EDGE('',*,*,#5890,.T.);
#8200=ORIENTED_EDGE('',*,*,#5885,.T.);
#8201=ORIENTED_EDGE('',*,*,#5880,.T.);
#8202=ORIENTED_EDGE('',*,*,#5875,.T.);
#8203=ORIENTED_EDGE('',*,*,#5864,.T.);
#8204=ORIENTED_EDGE('',*,*,#5874,.F.);
#8205=ORIENTED_EDGE('',*,*,#5879,.F.);
#8206=ORIENTED_EDGE('',*,*,#5884,.F.);
#8207=ORIENTED_EDGE('',*,*,#5889,.F.);
#8208=ORIENTED_EDGE('',*,*,#5894,.F.);
#8209=ORIENTED_EDGE('',*,*,#5899,.F.);
#8210=ORIENTED_EDGE('',*,*,#5933,.F.);
#8211=ORIENTED_EDGE('',*,*,#6264,.F.);
#8212=ORIENTED_EDGE('',*,*,#6234,.F.);
#8213=ORIENTED_EDGE('',*,*,#5862,.F.);
#8214=ORIENTED_EDGE('',*,*,#6009,.F.);
#8215=ORIENTED_EDGE('',*,*,#6265,.F.);
#8216=ORIENTED_EDGE('',*,*,#6232,.F.);
#8217=ORIENTED_EDGE('',*,*,#6266,.F.);
#8218=ORIENTED_EDGE('',*,*,#6231,.F.);
#8219=ORIENTED_EDGE('',*,*,#5863,.F.);
#8220=ORIENTED_EDGE('',*,*,#6233,.F.);
#8221=ORIENTED_EDGE('',*,*,#6267,.F.);
#8222=ORIENTED_EDGE('',*,*,#5968,.F.);
#8223=ORIENTED_EDGE('',*,*,#6268,.F.);
#8224=ORIENTED_EDGE('',*,*,#6269,.F.);
#8225=ORIENTED_EDGE('',*,*,#6270,.F.);
#8226=ORIENTED_EDGE('',*,*,#6271,.F.);
#8227=ORIENTED_EDGE('',*,*,#6272,.F.);
#8228=ORIENTED_EDGE('',*,*,#6273,.F.);
#8229=ORIENTED_EDGE('',*,*,#6264,.T.);
#8230=ORIENTED_EDGE('',*,*,#6008,.T.);
#8231=ORIENTED_EDGE('',*,*,#6274,.F.);
#8232=ORIENTED_EDGE('',*,*,#6266,.T.);
#8233=ORIENTED_EDGE('',*,*,#6267,.T.);
#8234=ORIENTED_EDGE('',*,*,#6265,.T.);
#8235=ORIENTED_EDGE('',*,*,#6275,.F.);
#8236=ORIENTED_EDGE('',*,*,#5969,.F.);
#8237=ORIENTED_EDGE('',*,*,#5861,.T.);
#8238=ORIENTED_EDGE('',*,*,#5987,.F.);
#8239=ORIENTED_EDGE('',*,*,#6276,.F.);
#8240=ORIENTED_EDGE('',*,*,#6010,.F.);
#8241=ORIENTED_EDGE('',*,*,#6272,.T.);
#8242=ORIENTED_EDGE('',*,*,#6011,.F.);
#8243=ORIENTED_EDGE('',*,*,#6277,.F.);
#8244=ORIENTED_EDGE('',*,*,#6224,.F.);
#8245=ORIENTED_EDGE('',*,*,#6273,.T.);
#8246=ORIENTED_EDGE('',*,*,#6227,.F.);
#8247=ORIENTED_EDGE('',*,*,#6278,.F.);
#8248=ORIENTED_EDGE('',*,*,#6253,.F.);
#8249=ORIENTED_EDGE('',*,*,#6269,.T.);
#8250=ORIENTED_EDGE('',*,*,#6254,.F.);
#8251=ORIENTED_EDGE('',*,*,#6279,.F.);
#8252=ORIENTED_EDGE('',*,*,#5993,.F.);
#8253=ORIENTED_EDGE('',*,*,#6270,.T.);
#8254=ORIENTED_EDGE('',*,*,#5992,.F.);
#8255=ORIENTED_EDGE('',*,*,#6280,.F.);
#8256=ORIENTED_EDGE('',*,*,#6218,.F.);
#8257=ORIENTED_EDGE('',*,*,#6268,.T.);
#8258=ORIENTED_EDGE('',*,*,#6217,.F.);
#8259=ORIENTED_EDGE('',*,*,#6281,.F.);
#8260=ORIENTED_EDGE('',*,*,#6255,.F.);
#8261=ORIENTED_EDGE('',*,*,#6271,.T.);
#8262=ORIENTED_EDGE('',*,*,#6252,.F.);
#8263=ORIENTED_EDGE('',*,*,#6282,.F.);
#8264=ORIENTED_EDGE('',*,*,#5994,.F.);
#8265=ORIENTED_EDGE('',*,*,#6274,.T.);
#8266=ORIENTED_EDGE('',*,*,#6007,.F.);
#8267=ORIENTED_EDGE('',*,*,#6283,.F.);
#8268=ORIENTED_EDGE('',*,*,#6228,.F.);
#8269=ORIENTED_EDGE('',*,*,#6284,.F.);
#8270=ORIENTED_EDGE('',*,*,#6229,.F.);
#8271=ORIENTED_EDGE('',*,*,#6285,.F.);
#8272=ORIENTED_EDGE('',*,*,#6237,.F.);
#8273=ORIENTED_EDGE('',*,*,#6275,.T.);
#8274=ORIENTED_EDGE('',*,*,#6230,.F.);
#8275=ORIENTED_EDGE('',*,*,#6286,.F.);
#8276=ORIENTED_EDGE('',*,*,#5970,.F.);
#8277=ORIENTED_EDGE('',*,*,#6276,.T.);
#8278=ORIENTED_EDGE('',*,*,#5986,.T.);
#8279=ORIENTED_EDGE('',*,*,#6287,.F.);
#8280=ORIENTED_EDGE('',*,*,#6277,.T.);
#8281=ORIENTED_EDGE('',*,*,#6279,.T.);
#8282=ORIENTED_EDGE('',*,*,#6278,.T.);
#8283=ORIENTED_EDGE('',*,*,#6288,.F.);
#8284=ORIENTED_EDGE('',*,*,#6289,.F.);
#8285=ORIENTED_EDGE('',*,*,#6280,.T.);
#8286=ORIENTED_EDGE('',*,*,#6290,.F.);
#8287=ORIENTED_EDGE('',*,*,#6282,.T.);
#8288=ORIENTED_EDGE('',*,*,#6281,.T.);
#8289=ORIENTED_EDGE('',*,*,#6291,.F.);
#8290=ORIENTED_EDGE('',*,*,#6283,.T.);
#8291=ORIENTED_EDGE('',*,*,#6006,.T.);
#8292=ORIENTED_EDGE('',*,*,#6292,.F.);
#8293=ORIENTED_EDGE('',*,*,#6285,.T.);
#8294=ORIENTED_EDGE('',*,*,#6286,.T.);
#8295=ORIENTED_EDGE('',*,*,#6284,.T.);
#8296=ORIENTED_EDGE('',*,*,#6293,.F.);
#8297=ORIENTED_EDGE('',*,*,#5971,.F.);
#8298=ORIENTED_EDGE('',*,*,#6287,.T.);
#8299=ORIENTED_EDGE('',*,*,#5985,.F.);
#8300=ORIENTED_EDGE('',*,*,#6294,.F.);
#8301=ORIENTED_EDGE('',*,*,#6225,.F.);
#8302=ORIENTED_EDGE('',*,*,#6288,.T.);
#8303=ORIENTED_EDGE('',*,*,#6226,.F.);
#8304=ORIENTED_EDGE('',*,*,#6295,.F.);
#8305=ORIENTED_EDGE('',*,*,#5988,.F.);
#8306=ORIENTED_EDGE('',*,*,#6290,.T.);
#8307=ORIENTED_EDGE('',*,*,#5991,.F.);
#8308=ORIENTED_EDGE('',*,*,#6296,.F.);
#8309=ORIENTED_EDGE('',*,*,#6250,.F.);
#8310=ORIENTED_EDGE('',*,*,#6289,.T.);
#8311=ORIENTED_EDGE('',*,*,#6249,.F.);
#8312=ORIENTED_EDGE('',*,*,#6297,.F.);
#8313=ORIENTED_EDGE('',*,*,#6219,.F.);
#8314=ORIENTED_EDGE('',*,*,#6291,.T.);
#8315=ORIENTED_EDGE('',*,*,#6216,.F.);
#8316=ORIENTED_EDGE('',*,*,#6298,.F.);
#8317=ORIENTED_EDGE('',*,*,#5995,.F.);
#8318=ORIENTED_EDGE('',*,*,#6292,.T.);
#8319=ORIENTED_EDGE('',*,*,#6005,.F.);
#8320=ORIENTED_EDGE('',*,*,#5859,.F.);
#8321=ORIENTED_EDGE('',*,*,#6235,.F.);
#8322=ORIENTED_EDGE('',*,*,#6293,.T.);
#8323=ORIENTED_EDGE('',*,*,#6236,.F.);
#8324=ORIENTED_EDGE('',*,*,#5858,.F.);
#8325=ORIENTED_EDGE('',*,*,#5972,.F.);
#8326=ORIENTED_EDGE('',*,*,#6294,.T.);
#8327=ORIENTED_EDGE('',*,*,#5984,.F.);
#8328=ORIENTED_EDGE('',*,*,#6299,.F.);
#8329=ORIENTED_EDGE('',*,*,#6295,.T.);
#8330=ORIENTED_EDGE('',*,*,#6300,.F.);
#8331=ORIENTED_EDGE('',*,*,#6296,.T.);
#8332=ORIENTED_EDGE('',*,*,#6301,.F.);
#8333=ORIENTED_EDGE('',*,*,#6298,.T.);
#8334=ORIENTED_EDGE('',*,*,#6297,.T.);
#8335=ORIENTED_EDGE('',*,*,#6302,.F.);
#8336=ORIENTED_EDGE('',*,*,#6299,.T.);
#8337=ORIENTED_EDGE('',*,*,#5983,.F.);
#8338=ORIENTED_EDGE('',*,*,#6303,.F.);
#8339=ORIENTED_EDGE('',*,*,#5989,.F.);
#8340=ORIENTED_EDGE('',*,*,#6301,.T.);
#8341=ORIENTED_EDGE('',*,*,#5990,.F.);
#8342=ORIENTED_EDGE('',*,*,#6304,.F.);
#8343=ORIENTED_EDGE('',*,*,#6221,.F.);
#8344=ORIENTED_EDGE('',*,*,#6300,.T.);
#8345=ORIENTED_EDGE('',*,*,#6220,.F.);
#8346=ORIENTED_EDGE('',*,*,#6305,.F.);
#8347=ORIENTED_EDGE('',*,*,#6251,.F.);
#8348=ORIENTED_EDGE('',*,*,#6302,.T.);
#8349=ORIENTED_EDGE('',*,*,#6248,.F.);
#8350=ORIENTED_EDGE('',*,*,#6306,.F.);
#8351=ORIENTED_EDGE('',*,*,#5996,.F.);
#8352=ORIENTED_EDGE('',*,*,#5856,.F.);
#8353=ORIENTED_EDGE('',*,*,#6003,.F.);
#8354=ORIENTED_EDGE('',*,*,#6307,.F.);
#8355=ORIENTED_EDGE('',*,*,#6247,.F.);
#8356=ORIENTED_EDGE('',*,*,#5860,.T.);
#8357=ORIENTED_EDGE('',*,*,#6004,.F.);
#8358=ORIENTED_EDGE('',*,*,#5855,.F.);
#8359=ORIENTED_EDGE('',*,*,#5973,.F.);
#8360=ORIENTED_EDGE('',*,*,#6303,.T.);
#8361=ORIENTED_EDGE('',*,*,#5982,.F.);
#8362=ORIENTED_EDGE('',*,*,#6308,.F.);
#8363=ORIENTED_EDGE('',*,*,#6304,.T.);
#8364=ORIENTED_EDGE('',*,*,#6306,.T.);
#8365=ORIENTED_EDGE('',*,*,#6305,.T.);
#8366=ORIENTED_EDGE('',*,*,#6309,.F.);
#8367=ORIENTED_EDGE('',*,*,#6307,.T.);
#8368=ORIENTED_EDGE('',*,*,#6002,.T.);
#8369=ORIENTED_EDGE('',*,*,#6310,.F.);
#8370=ORIENTED_EDGE('',*,*,#6311,.F.);
#8371=ORIENTED_EDGE('',*,*,#6308,.T.);
#8372=ORIENTED_EDGE('',*,*,#5981,.F.);
#8373=ORIENTED_EDGE('',*,*,#6312,.F.);
#8374=ORIENTED_EDGE('',*,*,#6222,.F.);
#8375=ORIENTED_EDGE('',*,*,#6309,.T.);
#8376=ORIENTED_EDGE('',*,*,#6223,.F.);
#8377=ORIENTED_EDGE('',*,*,#6313,.F.);
#8378=ORIENTED_EDGE('',*,*,#5997,.F.);
#8379=ORIENTED_EDGE('',*,*,#6310,.T.);
#8380=ORIENTED_EDGE('',*,*,#6001,.F.);
#8381=ORIENTED_EDGE('',*,*,#6314,.F.);
#8382=ORIENTED_EDGE('',*,*,#6238,.F.);
#8383=ORIENTED_EDGE('',*,*,#6311,.T.);
#8384=ORIENTED_EDGE('',*,*,#6241,.F.);
#8385=ORIENTED_EDGE('',*,*,#6315,.F.);
#8386=ORIENTED_EDGE('',*,*,#6245,.F.);
#8387=ORIENTED_EDGE('',*,*,#5857,.T.);
#8388=ORIENTED_EDGE('',*,*,#6246,.F.);
#8389=ORIENTED_EDGE('',*,*,#6316,.F.);
#8390=ORIENTED_EDGE('',*,*,#5974,.F.);
#8391=ORIENTED_EDGE('',*,*,#6312,.T.);
#8392=ORIENTED_EDGE('',*,*,#5980,.T.);
#8393=ORIENTED_EDGE('',*,*,#6317,.F.);
#8394=ORIENTED_EDGE('',*,*,#6313,.T.);
#8395=ORIENTED_EDGE('',*,*,#6314,.T.);
#8396=ORIENTED_EDGE('',*,*,#6000,.T.);
#8397=ORIENTED_EDGE('',*,*,#6318,.F.);
#8398=ORIENTED_EDGE('',*,*,#6319,.F.);
#8399=ORIENTED_EDGE('',*,*,#6316,.T.);
#8400=ORIENTED_EDGE('',*,*,#6315,.T.);
#8401=ORIENTED_EDGE('',*,*,#6320,.F.);
#8402=ORIENTED_EDGE('',*,*,#5975,.F.);
#8403=ORIENTED_EDGE('',*,*,#6317,.T.);
#8404=ORIENTED_EDGE('',*,*,#5979,.F.);
#8405=ORIENTED_EDGE('',*,*,#5854,.F.);
#8406=ORIENTED_EDGE('',*,*,#5998,.F.);
#8407=ORIENTED_EDGE('',*,*,#6318,.T.);
#8408=ORIENTED_EDGE('',*,*,#5999,.F.);
#8409=ORIENTED_EDGE('',*,*,#5853,.F.);
#8410=ORIENTED_EDGE('',*,*,#6242,.F.);
#8411=ORIENTED_EDGE('',*,*,#6319,.T.);
#8412=ORIENTED_EDGE('',*,*,#6244,.F.);
#8413=ORIENTED_EDGE('',*,*,#6321,.F.);
#8414=ORIENTED_EDGE('',*,*,#6239,.F.);
#8415=ORIENTED_EDGE('',*,*,#6320,.T.);
#8416=ORIENTED_EDGE('',*,*,#6240,.F.);
#8417=ORIENTED_EDGE('',*,*,#6322,.F.);
#8418=ORIENTED_EDGE('',*,*,#5976,.F.);
#8419=ORIENTED_EDGE('',*,*,#6322,.T.);
#8420=ORIENTED_EDGE('',*,*,#6321,.T.);
#8421=ORIENTED_EDGE('',*,*,#6323,.F.);
#8422=ORIENTED_EDGE('',*,*,#5977,.F.);
#8423=ORIENTED_EDGE('',*,*,#5852,.T.);
#8424=ORIENTED_EDGE('',*,*,#5978,.F.);
#8425=ORIENTED_EDGE('',*,*,#6323,.T.);
#8426=ORIENTED_EDGE('',*,*,#6243,.F.);
#8427=ORIENTED_EDGE('',*,*,#6324,.F.);
#8428=ORIENTED_EDGE('',*,*,#6325,.F.);
#8429=ORIENTED_EDGE('',*,*,#6326,.F.);
#8430=ORIENTED_EDGE('',*,*,#6327,.F.);
#8431=ORIENTED_EDGE('',*,*,#6263,.F.);
#8432=ORIENTED_EDGE('',*,*,#6328,.F.);
#8433=ORIENTED_EDGE('',*,*,#6016,.F.);
#8434=ORIENTED_EDGE('',*,*,#6325,.T.);
#8435=ORIENTED_EDGE('',*,*,#6260,.F.);
#8436=ORIENTED_EDGE('',*,*,#6329,.F.);
#8437=ORIENTED_EDGE('',*,*,#6179,.F.);
#8438=ORIENTED_EDGE('',*,*,#6326,.T.);
#8439=ORIENTED_EDGE('',*,*,#6178,.F.);
#8440=ORIENTED_EDGE('',*,*,#6330,.F.);
#8441=ORIENTED_EDGE('',*,*,#6186,.F.);
#8442=ORIENTED_EDGE('',*,*,#6324,.T.);
#8443=ORIENTED_EDGE('',*,*,#6185,.F.);
#8444=ORIENTED_EDGE('',*,*,#6331,.F.);
#8445=ORIENTED_EDGE('',*,*,#6261,.F.);
#8446=ORIENTED_EDGE('',*,*,#6332,.F.);
#8447=ORIENTED_EDGE('',*,*,#6262,.F.);
#8448=ORIENTED_EDGE('',*,*,#6333,.F.);
#8449=ORIENTED_EDGE('',*,*,#6195,.F.);
#8450=ORIENTED_EDGE('',*,*,#6328,.T.);
#8451=ORIENTED_EDGE('',*,*,#6332,.T.);
#8452=ORIENTED_EDGE('',*,*,#6334,.F.);
#8453=ORIENTED_EDGE('',*,*,#6329,.T.);
#8454=ORIENTED_EDGE('',*,*,#6327,.T.);
#8455=ORIENTED_EDGE('',*,*,#6335,.F.);
#8456=ORIENTED_EDGE('',*,*,#6336,.F.);
#8457=ORIENTED_EDGE('',*,*,#6330,.T.);
#8458=ORIENTED_EDGE('',*,*,#6337,.F.);
#8459=ORIENTED_EDGE('',*,*,#6333,.T.);
#8460=ORIENTED_EDGE('',*,*,#6331,.T.);
#8461=ORIENTED_EDGE('',*,*,#6338,.F.);
#8462=ORIENTED_EDGE('',*,*,#6334,.T.);
#8463=ORIENTED_EDGE('',*,*,#6194,.F.);
#8464=ORIENTED_EDGE('',*,*,#6339,.F.);
#8465=ORIENTED_EDGE('',*,*,#6017,.F.);
#8466=ORIENTED_EDGE('',*,*,#6335,.T.);
#8467=ORIENTED_EDGE('',*,*,#6015,.F.);
#8468=ORIENTED_EDGE('',*,*,#6340,.F.);
#8469=ORIENTED_EDGE('',*,*,#6180,.F.);
#8470=ORIENTED_EDGE('',*,*,#6337,.T.);
#8471=ORIENTED_EDGE('',*,*,#6181,.F.);
#8472=ORIENTED_EDGE('',*,*,#6341,.F.);
#8473=ORIENTED_EDGE('',*,*,#6257,.F.);
#8474=ORIENTED_EDGE('',*,*,#6336,.T.);
#8475=ORIENTED_EDGE('',*,*,#6256,.F.);
#8476=ORIENTED_EDGE('',*,*,#6342,.F.);
#8477=ORIENTED_EDGE('',*,*,#6187,.F.);
#8478=ORIENTED_EDGE('',*,*,#6338,.T.);
#8479=ORIENTED_EDGE('',*,*,#6184,.F.);
#8480=ORIENTED_EDGE('',*,*,#6343,.F.);
#8481=ORIENTED_EDGE('',*,*,#6192,.F.);
#8482=ORIENTED_EDGE('',*,*,#6344,.F.);
#8483=ORIENTED_EDGE('',*,*,#5957,.F.);
#8484=ORIENTED_EDGE('',*,*,#6345,.F.);
#8485=ORIENTED_EDGE('',*,*,#6193,.F.);
#8486=ORIENTED_EDGE('',*,*,#6345,.T.);
#8487=ORIENTED_EDGE('',*,*,#5956,.T.);
#8488=ORIENTED_EDGE('',*,*,#5850,.F.);
#8489=ORIENTED_EDGE('',*,*,#6339,.T.);
#8490=ORIENTED_EDGE('',*,*,#6341,.T.);
#8491=ORIENTED_EDGE('',*,*,#6340,.T.);
#8492=ORIENTED_EDGE('',*,*,#6346,.F.);
#8493=ORIENTED_EDGE('',*,*,#6347,.F.);
#8494=ORIENTED_EDGE('',*,*,#6342,.T.);
#8495=ORIENTED_EDGE('',*,*,#6348,.F.);
#8496=ORIENTED_EDGE('',*,*,#6344,.T.);
#8497=ORIENTED_EDGE('',*,*,#6343,.T.);
#8498=ORIENTED_EDGE('',*,*,#6349,.F.);
#8499=ORIENTED_EDGE('',*,*,#5958,.F.);
#8500=ORIENTED_EDGE('',*,*,#6346,.T.);
#8501=ORIENTED_EDGE('',*,*,#6014,.F.);
#8502=ORIENTED_EDGE('',*,*,#6350,.F.);
#8503=ORIENTED_EDGE('',*,*,#6258,.F.);
#8504=ORIENTED_EDGE('',*,*,#6348,.T.);
#8505=ORIENTED_EDGE('',*,*,#6259,.F.);
#8506=ORIENTED_EDGE('',*,*,#6351,.F.);
#8507=ORIENTED_EDGE('',*,*,#6189,.F.);
#8508=ORIENTED_EDGE('',*,*,#6347,.T.);
#8509=ORIENTED_EDGE('',*,*,#6188,.F.);
#8510=ORIENTED_EDGE('',*,*,#6352,.F.);
#8511=ORIENTED_EDGE('',*,*,#6182,.F.);
#8512=ORIENTED_EDGE('',*,*,#6349,.T.);
#8513=ORIENTED_EDGE('',*,*,#6183,.F.);
#8514=ORIENTED_EDGE('',*,*,#6353,.F.);
#8515=ORIENTED_EDGE('',*,*,#5959,.F.);
#8516=ORIENTED_EDGE('',*,*,#6354,.F.);
#8517=ORIENTED_EDGE('',*,*,#5848,.T.);
#8518=ORIENTED_EDGE('',*,*,#6355,.F.);
#8519=ORIENTED_EDGE('',*,*,#6351,.T.);
#8520=ORIENTED_EDGE('',*,*,#6350,.T.);
#8521=ORIENTED_EDGE('',*,*,#6356,.F.);
#8522=ORIENTED_EDGE('',*,*,#6353,.T.);
#8523=ORIENTED_EDGE('',*,*,#6352,.T.);
#8524=ORIENTED_EDGE('',*,*,#6357,.F.);
#8525=ORIENTED_EDGE('',*,*,#5960,.F.);
#8526=ORIENTED_EDGE('',*,*,#6355,.T.);
#8527=ORIENTED_EDGE('',*,*,#5955,.F.);
#8528=ORIENTED_EDGE('',*,*,#6358,.F.);
#8529=ORIENTED_EDGE('',*,*,#6201,.F.);
#8530=ORIENTED_EDGE('',*,*,#6359,.F.);
#8531=ORIENTED_EDGE('',*,*,#6202,.F.);
#8532=ORIENTED_EDGE('',*,*,#6360,.F.);
#8533=ORIENTED_EDGE('',*,*,#6196,.F.);
#8534=ORIENTED_EDGE('',*,*,#6354,.T.);
#8535=ORIENTED_EDGE('',*,*,#6200,.F.);
#8536=ORIENTED_EDGE('',*,*,#6361,.F.);
#8537=ORIENTED_EDGE('',*,*,#6018,.F.);
#8538=ORIENTED_EDGE('',*,*,#6356,.T.);
#8539=ORIENTED_EDGE('',*,*,#6013,.F.);
#8540=ORIENTED_EDGE('',*,*,#6362,.F.);
#8541=ORIENTED_EDGE('',*,*,#6190,.F.);
#8542=ORIENTED_EDGE('',*,*,#6357,.T.);
#8543=ORIENTED_EDGE('',*,*,#6191,.F.);
#8544=ORIENTED_EDGE('',*,*,#6363,.F.);
#8545=ORIENTED_EDGE('',*,*,#5961,.F.);
#8546=ORIENTED_EDGE('',*,*,#6358,.T.);
#8547=ORIENTED_EDGE('',*,*,#5954,.F.);
#8548=ORIENTED_EDGE('',*,*,#6364,.F.);
#8549=ORIENTED_EDGE('',*,*,#6360,.T.);
#8550=ORIENTED_EDGE('',*,*,#6361,.T.);
#8551=ORIENTED_EDGE('',*,*,#6359,.T.);
#8552=ORIENTED_EDGE('',*,*,#6365,.F.);
#8553=ORIENTED_EDGE('',*,*,#6019,.T.);
#8554=ORIENTED_EDGE('',*,*,#6363,.T.);
#8555=ORIENTED_EDGE('',*,*,#6362,.T.);
#8556=ORIENTED_EDGE('',*,*,#5844,.F.);
#8557=ORIENTED_EDGE('',*,*,#5843,.F.);
#8558=ORIENTED_EDGE('',*,*,#5962,.T.);
#8559=ORIENTED_EDGE('',*,*,#6364,.T.);
#8560=ORIENTED_EDGE('',*,*,#5953,.F.);
#8561=ORIENTED_EDGE('',*,*,#6366,.F.);
#8562=ORIENTED_EDGE('',*,*,#6197,.F.);
#8563=ORIENTED_EDGE('',*,*,#6367,.F.);
#8564=ORIENTED_EDGE('',*,*,#6198,.F.);
#8565=ORIENTED_EDGE('',*,*,#6368,.F.);
#8566=ORIENTED_EDGE('',*,*,#6203,.F.);
#8567=ORIENTED_EDGE('',*,*,#6365,.T.);
#8568=ORIENTED_EDGE('',*,*,#6199,.F.);
#8569=ORIENTED_EDGE('',*,*,#6369,.F.);
#8570=ORIENTED_EDGE('',*,*,#6020,.F.);
#8571=ORIENTED_EDGE('',*,*,#6370,.F.);
#8572=ORIENTED_EDGE('',*,*,#6012,.F.);
#8573=ORIENTED_EDGE('',*,*,#6371,.F.);
#8574=ORIENTED_EDGE('',*,*,#6212,.F.);
#8575=ORIENTED_EDGE('',*,*,#6366,.T.);
#8576=ORIENTED_EDGE('',*,*,#5952,.F.);
#8577=ORIENTED_EDGE('',*,*,#6372,.F.);
#8578=ORIENTED_EDGE('',*,*,#6368,.T.);
#8579=ORIENTED_EDGE('',*,*,#6369,.T.);
#8580=ORIENTED_EDGE('',*,*,#6367,.T.);
#8581=ORIENTED_EDGE('',*,*,#6373,.F.);
#8582=ORIENTED_EDGE('',*,*,#6021,.T.);
#8583=ORIENTED_EDGE('',*,*,#6371,.T.);
#8584=ORIENTED_EDGE('',*,*,#6026,.T.);
#8585=ORIENTED_EDGE('',*,*,#6374,.F.);
#8586=ORIENTED_EDGE('',*,*,#6375,.F.);
#8587=ORIENTED_EDGE('',*,*,#5846,.T.);
#8588=ORIENTED_EDGE('',*,*,#6370,.T.);
#8589=ORIENTED_EDGE('',*,*,#6376,.F.);
#8590=ORIENTED_EDGE('',*,*,#6372,.T.);
#8591=ORIENTED_EDGE('',*,*,#5951,.F.);
#8592=ORIENTED_EDGE('',*,*,#6377,.F.);
#8593=ORIENTED_EDGE('',*,*,#6204,.F.);
#8594=ORIENTED_EDGE('',*,*,#6373,.T.);
#8595=ORIENTED_EDGE('',*,*,#6205,.F.);
#8596=ORIENTED_EDGE('',*,*,#6378,.F.);
#8597=ORIENTED_EDGE('',*,*,#6022,.F.);
#8598=ORIENTED_EDGE('',*,*,#6374,.T.);
#8599=ORIENTED_EDGE('',*,*,#6025,.F.);
#8600=ORIENTED_EDGE('',*,*,#6379,.F.);
#8601=ORIENTED_EDGE('',*,*,#6209,.F.);
#8602=ORIENTED_EDGE('',*,*,#6375,.T.);
#8603=ORIENTED_EDGE('',*,*,#6208,.F.);
#8604=ORIENTED_EDGE('',*,*,#6380,.F.);
#8605=ORIENTED_EDGE('',*,*,#6210,.F.);
#8606=ORIENTED_EDGE('',*,*,#6376,.T.);
#8607=ORIENTED_EDGE('',*,*,#6211,.F.);
#8608=ORIENTED_EDGE('',*,*,#6381,.F.);
#8609=ORIENTED_EDGE('',*,*,#5963,.F.);
#8610=ORIENTED_EDGE('',*,*,#6378,.T.);
#8611=ORIENTED_EDGE('',*,*,#6377,.T.);
#8612=ORIENTED_EDGE('',*,*,#5841,.F.);
#8613=ORIENTED_EDGE('',*,*,#6379,.T.);
#8614=ORIENTED_EDGE('',*,*,#6024,.T.);
#8615=ORIENTED_EDGE('',*,*,#6382,.F.);
#8616=ORIENTED_EDGE('',*,*,#6383,.F.);
#8617=ORIENTED_EDGE('',*,*,#6381,.T.);
#8618=ORIENTED_EDGE('',*,*,#6380,.T.);
#8619=ORIENTED_EDGE('',*,*,#6384,.F.);
#8620=ORIENTED_EDGE('',*,*,#5964,.F.);
#8621=ORIENTED_EDGE('',*,*,#6382,.T.);
#8622=ORIENTED_EDGE('',*,*,#6023,.F.);
#8623=ORIENTED_EDGE('',*,*,#6385,.F.);
#8624=ORIENTED_EDGE('',*,*,#6213,.F.);
#8625=ORIENTED_EDGE('',*,*,#6383,.T.);
#8626=ORIENTED_EDGE('',*,*,#6215,.F.);
#8627=ORIENTED_EDGE('',*,*,#6386,.F.);
#8628=ORIENTED_EDGE('',*,*,#6206,.F.);
#8629=ORIENTED_EDGE('',*,*,#6384,.T.);
#8630=ORIENTED_EDGE('',*,*,#6207,.F.);
#8631=ORIENTED_EDGE('',*,*,#6387,.F.);
#8632=ORIENTED_EDGE('',*,*,#5965,.F.);
#8633=ORIENTED_EDGE('',*,*,#6385,.T.);
#8634=ORIENTED_EDGE('',*,*,#5839,.T.);
#8635=ORIENTED_EDGE('',*,*,#6388,.F.);
#8636=ORIENTED_EDGE('',*,*,#6387,.T.);
#8637=ORIENTED_EDGE('',*,*,#6386,.T.);
#8638=ORIENTED_EDGE('',*,*,#6389,.F.);
#8639=ORIENTED_EDGE('',*,*,#5966,.F.);
#8640=ORIENTED_EDGE('',*,*,#6388,.T.);
#8641=ORIENTED_EDGE('',*,*,#5967,.F.);
#8642=ORIENTED_EDGE('',*,*,#6389,.T.);
#8643=ORIENTED_EDGE('',*,*,#6214,.F.);
#8644=ORIENTED_EDGE('',*,*,#6390,.F.);
#8645=ORIENTED_EDGE('',*,*,#6391,.T.);
#8646=ORIENTED_EDGE('',*,*,#6392,.F.);
#8647=ORIENTED_EDGE('',*,*,#6393,.F.);
#8648=ORIENTED_EDGE('',*,*,#6391,.F.);
#8649=ORIENTED_EDGE('',*,*,#6394,.F.);
#8650=ORIENTED_EDGE('',*,*,#6395,.F.);
#8651=ORIENTED_EDGE('',*,*,#6396,.T.);
#8652=ORIENTED_EDGE('',*,*,#6397,.F.);
#8653=ORIENTED_EDGE('',*,*,#6396,.F.);
#8654=ORIENTED_EDGE('',*,*,#6398,.F.);
#8655=ORIENTED_EDGE('',*,*,#6399,.F.);
#8656=ORIENTED_EDGE('',*,*,#6400,.T.);
#8657=ORIENTED_EDGE('',*,*,#6401,.F.);
#8658=ORIENTED_EDGE('',*,*,#6400,.F.);
#8659=ORIENTED_EDGE('',*,*,#6402,.T.);
#8660=ORIENTED_EDGE('',*,*,#6403,.T.);
#8661=ORIENTED_EDGE('',*,*,#6404,.T.);
#8662=ORIENTED_EDGE('',*,*,#6405,.F.);
#8663=ORIENTED_EDGE('',*,*,#6406,.T.);
#8664=ORIENTED_EDGE('',*,*,#6407,.T.);
#8665=ORIENTED_EDGE('',*,*,#6408,.F.);
#8666=ORIENTED_EDGE('',*,*,#6409,.F.);
#8667=ORIENTED_EDGE('',*,*,#6410,.F.);
#8668=ORIENTED_EDGE('',*,*,#6411,.F.);
#8669=ORIENTED_EDGE('',*,*,#6412,.F.);
#8670=ORIENTED_EDGE('',*,*,#6413,.F.);
#8671=ORIENTED_EDGE('',*,*,#6414,.F.);
#8672=ORIENTED_EDGE('',*,*,#6415,.F.);
#8673=ORIENTED_EDGE('',*,*,#6416,.F.);
#8674=ORIENTED_EDGE('',*,*,#6417,.F.);
#8675=ORIENTED_EDGE('',*,*,#6418,.F.);
#8676=ORIENTED_EDGE('',*,*,#6419,.F.);
#8677=ORIENTED_EDGE('',*,*,#6420,.F.);
#8678=ORIENTED_EDGE('',*,*,#6421,.F.);
#8679=ORIENTED_EDGE('',*,*,#6422,.F.);
#8680=ORIENTED_EDGE('',*,*,#6423,.F.);
#8681=ORIENTED_EDGE('',*,*,#6424,.F.);
#8682=ORIENTED_EDGE('',*,*,#6425,.T.);
#8683=ORIENTED_EDGE('',*,*,#6426,.F.);
#8684=ORIENTED_EDGE('',*,*,#6427,.F.);
#8685=ORIENTED_EDGE('',*,*,#6428,.F.);
#8686=ORIENTED_EDGE('',*,*,#6407,.F.);
#8687=ORIENTED_EDGE('',*,*,#6429,.T.);
#8688=ORIENTED_EDGE('',*,*,#6430,.T.);
#8689=ORIENTED_EDGE('',*,*,#6431,.F.);
#8690=ORIENTED_EDGE('',*,*,#6432,.F.);
#8691=ORIENTED_EDGE('',*,*,#6433,.T.);
#8692=ORIENTED_EDGE('',*,*,#6434,.T.);
#8693=ORIENTED_EDGE('',*,*,#6435,.F.);
#8694=ORIENTED_EDGE('',*,*,#6434,.F.);
#8695=ORIENTED_EDGE('',*,*,#6436,.T.);
#8696=ORIENTED_EDGE('',*,*,#6437,.T.);
#8697=ORIENTED_EDGE('',*,*,#6438,.F.);
#8698=ORIENTED_EDGE('',*,*,#6430,.F.);
#8699=ORIENTED_EDGE('',*,*,#6439,.T.);
#8700=ORIENTED_EDGE('',*,*,#6440,.T.);
#8701=ORIENTED_EDGE('',*,*,#6441,.F.);
#8702=ORIENTED_EDGE('',*,*,#6442,.F.);
#8703=ORIENTED_EDGE('',*,*,#6443,.F.);
#8704=ORIENTED_EDGE('',*,*,#6444,.T.);
#8705=ORIENTED_EDGE('',*,*,#6445,.T.);
#8706=ORIENTED_EDGE('',*,*,#6446,.F.);
#8707=ORIENTED_EDGE('',*,*,#6447,.F.);
#8708=ORIENTED_EDGE('',*,*,#6448,.T.);
#8709=ORIENTED_EDGE('',*,*,#6449,.T.);
#8710=ORIENTED_EDGE('',*,*,#6450,.F.);
#8711=ORIENTED_EDGE('',*,*,#6451,.F.);
#8712=ORIENTED_EDGE('',*,*,#6452,.T.);
#8713=ORIENTED_EDGE('',*,*,#6453,.T.);
#8714=ORIENTED_EDGE('',*,*,#6454,.F.);
#8715=ORIENTED_EDGE('',*,*,#6455,.F.);
#8716=ORIENTED_EDGE('',*,*,#6456,.T.);
#8717=ORIENTED_EDGE('',*,*,#6457,.T.);
#8718=ORIENTED_EDGE('',*,*,#6458,.F.);
#8719=ORIENTED_EDGE('',*,*,#6459,.T.);
#8720=ORIENTED_EDGE('',*,*,#6460,.T.);
#8721=ORIENTED_EDGE('',*,*,#6461,.F.);
#8722=ORIENTED_EDGE('',*,*,#6462,.F.);
#8723=ORIENTED_EDGE('',*,*,#6463,.F.);
#8724=ORIENTED_EDGE('',*,*,#6464,.T.);
#8725=ORIENTED_EDGE('',*,*,#6465,.T.);
#8726=ORIENTED_EDGE('',*,*,#6466,.F.);
#8727=ORIENTED_EDGE('',*,*,#6467,.F.);
#8728=ORIENTED_EDGE('',*,*,#6468,.T.);
#8729=ORIENTED_EDGE('',*,*,#6469,.T.);
#8730=ORIENTED_EDGE('',*,*,#6470,.F.);
#8731=ORIENTED_EDGE('',*,*,#6471,.F.);
#8732=ORIENTED_EDGE('',*,*,#6472,.T.);
#8733=ORIENTED_EDGE('',*,*,#6473,.T.);
#8734=ORIENTED_EDGE('',*,*,#6474,.F.);
#8735=ORIENTED_EDGE('',*,*,#6398,.T.);
#8736=ORIENTED_EDGE('',*,*,#6399,.T.);
#8737=ORIENTED_EDGE('',*,*,#6475,.T.);
#8738=ORIENTED_EDGE('',*,*,#6392,.T.);
#8739=ORIENTED_EDGE('',*,*,#6393,.T.);
#8740=ORIENTED_EDGE('',*,*,#6475,.F.);
#8741=ORIENTED_EDGE('',*,*,#6394,.T.);
#8742=ORIENTED_EDGE('',*,*,#6395,.T.);
#8743=ORIENTED_EDGE('',*,*,#6476,.T.);
#8744=ORIENTED_EDGE('',*,*,#6477,.F.);
#8745=ORIENTED_EDGE('',*,*,#6476,.F.);
#8746=ORIENTED_EDGE('',*,*,#6423,.T.);
#8747=ORIENTED_EDGE('',*,*,#6478,.T.);
#8748=ORIENTED_EDGE('',*,*,#6479,.T.);
#8749=ORIENTED_EDGE('',*,*,#6480,.T.);
#8750=ORIENTED_EDGE('',*,*,#6421,.T.);
#8751=ORIENTED_EDGE('',*,*,#6481,.T.);
#8752=ORIENTED_EDGE('',*,*,#6482,.T.);
#8753=ORIENTED_EDGE('',*,*,#6483,.T.);
#8754=ORIENTED_EDGE('',*,*,#6419,.T.);
#8755=ORIENTED_EDGE('',*,*,#6484,.T.);
#8756=ORIENTED_EDGE('',*,*,#6485,.T.);
#8757=ORIENTED_EDGE('',*,*,#6486,.T.);
#8758=ORIENTED_EDGE('',*,*,#6417,.T.);
#8759=ORIENTED_EDGE('',*,*,#6487,.T.);
#8760=ORIENTED_EDGE('',*,*,#6488,.T.);
#8761=ORIENTED_EDGE('',*,*,#6489,.T.);
#8762=ORIENTED_EDGE('',*,*,#6415,.T.);
#8763=ORIENTED_EDGE('',*,*,#6490,.T.);
#8764=ORIENTED_EDGE('',*,*,#6491,.T.);
#8765=ORIENTED_EDGE('',*,*,#6492,.T.);
#8766=ORIENTED_EDGE('',*,*,#6413,.T.);
#8767=ORIENTED_EDGE('',*,*,#6493,.T.);
#8768=ORIENTED_EDGE('',*,*,#6494,.T.);
#8769=ORIENTED_EDGE('',*,*,#6495,.T.);
#8770=ORIENTED_EDGE('',*,*,#6411,.T.);
#8771=ORIENTED_EDGE('',*,*,#6496,.T.);
#8772=ORIENTED_EDGE('',*,*,#6497,.T.);
#8773=ORIENTED_EDGE('',*,*,#6498,.T.);
#8774=ORIENTED_EDGE('',*,*,#6409,.T.);
#8775=ORIENTED_EDGE('',*,*,#6499,.T.);
#8776=ORIENTED_EDGE('',*,*,#6500,.T.);
#8777=ORIENTED_EDGE('',*,*,#6501,.T.);
#8778=ORIENTED_EDGE('',*,*,#6427,.T.);
#8779=ORIENTED_EDGE('',*,*,#6502,.T.);
#8780=ORIENTED_EDGE('',*,*,#6503,.T.);
#8781=ORIENTED_EDGE('',*,*,#6504,.T.);
#8782=ORIENTED_EDGE('',*,*,#6425,.F.);
#8783=ORIENTED_EDGE('',*,*,#6505,.T.);
#8784=ORIENTED_EDGE('',*,*,#6506,.T.);
#8785=ORIENTED_EDGE('',*,*,#6507,.T.);
#8786=ORIENTED_EDGE('',*,*,#6466,.T.);
#8787=ORIENTED_EDGE('',*,*,#6508,.F.);
#8788=ORIENTED_EDGE('',*,*,#6509,.F.);
#8789=ORIENTED_EDGE('',*,*,#6510,.F.);
#8790=ORIENTED_EDGE('',*,*,#6511,.F.);
#8791=ORIENTED_EDGE('',*,*,#6512,.F.);
#8792=ORIENTED_EDGE('',*,*,#6461,.T.);
#8793=ORIENTED_EDGE('',*,*,#6513,.F.);
#8794=ORIENTED_EDGE('',*,*,#6514,.F.);
#8795=ORIENTED_EDGE('',*,*,#6515,.F.);
#8796=ORIENTED_EDGE('',*,*,#6516,.F.);
#8797=ORIENTED_EDGE('',*,*,#6517,.F.);
#8798=ORIENTED_EDGE('',*,*,#6474,.T.);
#8799=ORIENTED_EDGE('',*,*,#6518,.F.);
#8800=ORIENTED_EDGE('',*,*,#6519,.F.);
#8801=ORIENTED_EDGE('',*,*,#6520,.F.);
#8802=ORIENTED_EDGE('',*,*,#6521,.F.);
#8803=ORIENTED_EDGE('',*,*,#6522,.F.);
#8804=ORIENTED_EDGE('',*,*,#6470,.T.);
#8805=ORIENTED_EDGE('',*,*,#6523,.F.);
#8806=ORIENTED_EDGE('',*,*,#6524,.F.);
#8807=ORIENTED_EDGE('',*,*,#6525,.F.);
#8808=ORIENTED_EDGE('',*,*,#6526,.F.);
#8809=ORIENTED_EDGE('',*,*,#6527,.F.);
#8810=ORIENTED_EDGE('',*,*,#6441,.T.);
#8811=ORIENTED_EDGE('',*,*,#6528,.F.);
#8812=ORIENTED_EDGE('',*,*,#6529,.F.);
#8813=ORIENTED_EDGE('',*,*,#6530,.F.);
#8814=ORIENTED_EDGE('',*,*,#6531,.F.);
#8815=ORIENTED_EDGE('',*,*,#6532,.F.);
#8816=ORIENTED_EDGE('',*,*,#6458,.T.);
#8817=ORIENTED_EDGE('',*,*,#6533,.F.);
#8818=ORIENTED_EDGE('',*,*,#6534,.F.);
#8819=ORIENTED_EDGE('',*,*,#6535,.F.);
#8820=ORIENTED_EDGE('',*,*,#6536,.F.);
#8821=ORIENTED_EDGE('',*,*,#6537,.F.);
#8822=ORIENTED_EDGE('',*,*,#6454,.T.);
#8823=ORIENTED_EDGE('',*,*,#6538,.F.);
#8824=ORIENTED_EDGE('',*,*,#6539,.F.);
#8825=ORIENTED_EDGE('',*,*,#6540,.F.);
#8826=ORIENTED_EDGE('',*,*,#6541,.F.);
#8827=ORIENTED_EDGE('',*,*,#6542,.F.);
#8828=ORIENTED_EDGE('',*,*,#6450,.T.);
#8829=ORIENTED_EDGE('',*,*,#6543,.F.);
#8830=ORIENTED_EDGE('',*,*,#6544,.F.);
#8831=ORIENTED_EDGE('',*,*,#6545,.F.);
#8832=ORIENTED_EDGE('',*,*,#6546,.F.);
#8833=ORIENTED_EDGE('',*,*,#6547,.F.);
#8834=ORIENTED_EDGE('',*,*,#6446,.T.);
#8835=ORIENTED_EDGE('',*,*,#6548,.F.);
#8836=ORIENTED_EDGE('',*,*,#6549,.F.);
#8837=ORIENTED_EDGE('',*,*,#6550,.F.);
#8838=ORIENTED_EDGE('',*,*,#6551,.F.);
#8839=ORIENTED_EDGE('',*,*,#6552,.F.);
#8840=ORIENTED_EDGE('',*,*,#6431,.T.);
#8841=ORIENTED_EDGE('',*,*,#6438,.T.);
#8842=ORIENTED_EDGE('',*,*,#6553,.F.);
#8843=ORIENTED_EDGE('',*,*,#6554,.F.);
#8844=ORIENTED_EDGE('',*,*,#6555,.F.);
#8845=ORIENTED_EDGE('',*,*,#6556,.F.);
#8846=ORIENTED_EDGE('',*,*,#6557,.F.);
#8847=ORIENTED_EDGE('',*,*,#6558,.F.);
#8848=ORIENTED_EDGE('',*,*,#6402,.F.);
#8849=ORIENTED_EDGE('',*,*,#6559,.F.);
#8850=ORIENTED_EDGE('',*,*,#6560,.F.);
#8851=ORIENTED_EDGE('',*,*,#6397,.T.);
#8852=ORIENTED_EDGE('',*,*,#6404,.F.);
#8853=ORIENTED_EDGE('',*,*,#6561,.F.);
#8854=ORIENTED_EDGE('',*,*,#6562,.F.);
#8855=ORIENTED_EDGE('',*,*,#6563,.F.);
#8856=ORIENTED_EDGE('',*,*,#6401,.T.);
#8857=ORIENTED_EDGE('',*,*,#6477,.T.);
#8858=ORIENTED_EDGE('',*,*,#6429,.F.);
#8859=ORIENTED_EDGE('',*,*,#6390,.T.);
#8860=ORIENTED_EDGE('',*,*,#6564,.F.);
#8861=ORIENTED_EDGE('',*,*,#6565,.T.);
#8862=ORIENTED_EDGE('',*,*,#6566,.T.);
#8863=ORIENTED_EDGE('',*,*,#6516,.T.);
#8864=ORIENTED_EDGE('',*,*,#6480,.F.);
#8865=ORIENTED_EDGE('',*,*,#6567,.T.);
#8866=ORIENTED_EDGE('',*,*,#6564,.T.);
#8867=ORIENTED_EDGE('',*,*,#6515,.T.);
#8868=ORIENTED_EDGE('',*,*,#6568,.F.);
#8869=ORIENTED_EDGE('',*,*,#6569,.F.);
#8870=ORIENTED_EDGE('',*,*,#6514,.T.);
#8871=ORIENTED_EDGE('',*,*,#6570,.F.);
#8872=ORIENTED_EDGE('',*,*,#6571,.F.);
#8873=ORIENTED_EDGE('',*,*,#6568,.T.);
#8874=ORIENTED_EDGE('',*,*,#6513,.T.);
#8875=ORIENTED_EDGE('',*,*,#6460,.F.);
#8876=ORIENTED_EDGE('',*,*,#6572,.F.);
#8877=ORIENTED_EDGE('',*,*,#6570,.T.);
#8878=ORIENTED_EDGE('',*,*,#6566,.F.);
#8879=ORIENTED_EDGE('',*,*,#6573,.T.);
#8880=ORIENTED_EDGE('',*,*,#6478,.F.);
#8881=ORIENTED_EDGE('',*,*,#6574,.F.);
#8882=ORIENTED_EDGE('',*,*,#6471,.T.);
#8883=ORIENTED_EDGE('',*,*,#6517,.T.);
#8884=ORIENTED_EDGE('',*,*,#6573,.F.);
#8885=ORIENTED_EDGE('',*,*,#6565,.F.);
#8886=ORIENTED_EDGE('',*,*,#6567,.F.);
#8887=ORIENTED_EDGE('',*,*,#6479,.F.);
#8888=ORIENTED_EDGE('',*,*,#6575,.F.);
#8889=ORIENTED_EDGE('',*,*,#6576,.T.);
#8890=ORIENTED_EDGE('',*,*,#6577,.T.);
#8891=ORIENTED_EDGE('',*,*,#6521,.T.);
#8892=ORIENTED_EDGE('',*,*,#6483,.F.);
#8893=ORIENTED_EDGE('',*,*,#6578,.T.);
#8894=ORIENTED_EDGE('',*,*,#6575,.T.);
#8895=ORIENTED_EDGE('',*,*,#6520,.T.);
#8896=ORIENTED_EDGE('',*,*,#6579,.F.);
#8897=ORIENTED_EDGE('',*,*,#6580,.F.);
#8898=ORIENTED_EDGE('',*,*,#6519,.T.);
#8899=ORIENTED_EDGE('',*,*,#6581,.F.);
#8900=ORIENTED_EDGE('',*,*,#6582,.F.);
#8901=ORIENTED_EDGE('',*,*,#6579,.T.);
#8902=ORIENTED_EDGE('',*,*,#6518,.T.);
#8903=ORIENTED_EDGE('',*,*,#6473,.F.);
#8904=ORIENTED_EDGE('',*,*,#6583,.F.);
#8905=ORIENTED_EDGE('',*,*,#6581,.T.);
#8906=ORIENTED_EDGE('',*,*,#6577,.F.);
#8907=ORIENTED_EDGE('',*,*,#6584,.T.);
#8908=ORIENTED_EDGE('',*,*,#6481,.F.);
#8909=ORIENTED_EDGE('',*,*,#6585,.F.);
#8910=ORIENTED_EDGE('',*,*,#6467,.T.);
#8911=ORIENTED_EDGE('',*,*,#6522,.T.);
#8912=ORIENTED_EDGE('',*,*,#6586,.F.);
#8913=ORIENTED_EDGE('',*,*,#6587,.T.);
#8914=ORIENTED_EDGE('',*,*,#6588,.T.);
#8915=ORIENTED_EDGE('',*,*,#6526,.T.);
#8916=ORIENTED_EDGE('',*,*,#6486,.F.);
#8917=ORIENTED_EDGE('',*,*,#6589,.T.);
#8918=ORIENTED_EDGE('',*,*,#6586,.T.);
#8919=ORIENTED_EDGE('',*,*,#6525,.T.);
#8920=ORIENTED_EDGE('',*,*,#6590,.F.);
#8921=ORIENTED_EDGE('',*,*,#6591,.F.);
#8922=ORIENTED_EDGE('',*,*,#6524,.T.);
#8923=ORIENTED_EDGE('',*,*,#6592,.F.);
#8924=ORIENTED_EDGE('',*,*,#6593,.F.);
#8925=ORIENTED_EDGE('',*,*,#6590,.T.);
#8926=ORIENTED_EDGE('',*,*,#6523,.T.);
#8927=ORIENTED_EDGE('',*,*,#6469,.F.);
#8928=ORIENTED_EDGE('',*,*,#6594,.F.);
#8929=ORIENTED_EDGE('',*,*,#6592,.T.);
#8930=ORIENTED_EDGE('',*,*,#6588,.F.);
#8931=ORIENTED_EDGE('',*,*,#6595,.T.);
#8932=ORIENTED_EDGE('',*,*,#6484,.F.);
#8933=ORIENTED_EDGE('',*,*,#6596,.F.);
#8934=ORIENTED_EDGE('',*,*,#6442,.T.);
#8935=ORIENTED_EDGE('',*,*,#6527,.T.);
#8936=ORIENTED_EDGE('',*,*,#6597,.F.);
#8937=ORIENTED_EDGE('',*,*,#6598,.T.);
#8938=ORIENTED_EDGE('',*,*,#6599,.T.);
#8939=ORIENTED_EDGE('',*,*,#6531,.T.);
#8940=ORIENTED_EDGE('',*,*,#6489,.F.);
#8941=ORIENTED_EDGE('',*,*,#6600,.T.);
#8942=ORIENTED_EDGE('',*,*,#6597,.T.);
#8943=ORIENTED_EDGE('',*,*,#6530,.T.);
#8944=ORIENTED_EDGE('',*,*,#6601,.F.);
#8945=ORIENTED_EDGE('',*,*,#6602,.F.);
#8946=ORIENTED_EDGE('',*,*,#6529,.T.);
#8947=ORIENTED_EDGE('',*,*,#6603,.F.);
#8948=ORIENTED_EDGE('',*,*,#6604,.F.);
#8949=ORIENTED_EDGE('',*,*,#6601,.T.);
#8950=ORIENTED_EDGE('',*,*,#6528,.T.);
#8951=ORIENTED_EDGE('',*,*,#6440,.F.);
#8952=ORIENTED_EDGE('',*,*,#6605,.F.);
#8953=ORIENTED_EDGE('',*,*,#6603,.T.);
#8954=ORIENTED_EDGE('',*,*,#6599,.F.);
#8955=ORIENTED_EDGE('',*,*,#6606,.T.);
#8956=ORIENTED_EDGE('',*,*,#6487,.F.);
#8957=ORIENTED_EDGE('',*,*,#6607,.F.);
#8958=ORIENTED_EDGE('',*,*,#6455,.T.);
#8959=ORIENTED_EDGE('',*,*,#6532,.T.);
#8960=ORIENTED_EDGE('',*,*,#6608,.F.);
#8961=ORIENTED_EDGE('',*,*,#6609,.T.);
#8962=ORIENTED_EDGE('',*,*,#6610,.T.);
#8963=ORIENTED_EDGE('',*,*,#6536,.T.);
#8964=ORIENTED_EDGE('',*,*,#6492,.F.);
#8965=ORIENTED_EDGE('',*,*,#6611,.T.);
#8966=ORIENTED_EDGE('',*,*,#6608,.T.);
#8967=ORIENTED_EDGE('',*,*,#6535,.T.);
#8968=ORIENTED_EDGE('',*,*,#6612,.F.);
#8969=ORIENTED_EDGE('',*,*,#6613,.F.);
#8970=ORIENTED_EDGE('',*,*,#6534,.T.);
#8971=ORIENTED_EDGE('',*,*,#6614,.F.);
#8972=ORIENTED_EDGE('',*,*,#6615,.F.);
#8973=ORIENTED_EDGE('',*,*,#6612,.T.);
#8974=ORIENTED_EDGE('',*,*,#6533,.T.);
#8975=ORIENTED_EDGE('',*,*,#6457,.F.);
#8976=ORIENTED_EDGE('',*,*,#6616,.F.);
#8977=ORIENTED_EDGE('',*,*,#6614,.T.);
#8978=ORIENTED_EDGE('',*,*,#6610,.F.);
#8979=ORIENTED_EDGE('',*,*,#6617,.T.);
#8980=ORIENTED_EDGE('',*,*,#6490,.F.);
#8981=ORIENTED_EDGE('',*,*,#6618,.F.);
#8982=ORIENTED_EDGE('',*,*,#6451,.T.);
#8983=ORIENTED_EDGE('',*,*,#6537,.T.);
#8984=ORIENTED_EDGE('',*,*,#6619,.F.);
#8985=ORIENTED_EDGE('',*,*,#6620,.T.);
#8986=ORIENTED_EDGE('',*,*,#6621,.T.);
#8987=ORIENTED_EDGE('',*,*,#6541,.T.);
#8988=ORIENTED_EDGE('',*,*,#6495,.F.);
#8989=ORIENTED_EDGE('',*,*,#6622,.T.);
#8990=ORIENTED_EDGE('',*,*,#6619,.T.);
#8991=ORIENTED_EDGE('',*,*,#6540,.T.);
#8992=ORIENTED_EDGE('',*,*,#6623,.F.);
#8993=ORIENTED_EDGE('',*,*,#6624,.F.);
#8994=ORIENTED_EDGE('',*,*,#6539,.T.);
#8995=ORIENTED_EDGE('',*,*,#6625,.F.);
#8996=ORIENTED_EDGE('',*,*,#6626,.F.);
#8997=ORIENTED_EDGE('',*,*,#6623,.T.);
#8998=ORIENTED_EDGE('',*,*,#6538,.T.);
#8999=ORIENTED_EDGE('',*,*,#6453,.F.);
#9000=ORIENTED_EDGE('',*,*,#6627,.F.);
#9001=ORIENTED_EDGE('',*,*,#6625,.T.);
#9002=ORIENTED_EDGE('',*,*,#6621,.F.);
#9003=ORIENTED_EDGE('',*,*,#6628,.T.);
#9004=ORIENTED_EDGE('',*,*,#6493,.F.);
#9005=ORIENTED_EDGE('',*,*,#6629,.F.);
#9006=ORIENTED_EDGE('',*,*,#6447,.T.);
#9007=ORIENTED_EDGE('',*,*,#6542,.T.);
#9008=ORIENTED_EDGE('',*,*,#6630,.F.);
#9009=ORIENTED_EDGE('',*,*,#6631,.T.);
#9010=ORIENTED_EDGE('',*,*,#6632,.T.);
#9011=ORIENTED_EDGE('',*,*,#6546,.T.);
#9012=ORIENTED_EDGE('',*,*,#6498,.F.);
#9013=ORIENTED_EDGE('',*,*,#6633,.T.);
#9014=ORIENTED_EDGE('',*,*,#6630,.T.);
#9015=ORIENTED_EDGE('',*,*,#6545,.T.);
#9016=ORIENTED_EDGE('',*,*,#6634,.F.);
#9017=ORIENTED_EDGE('',*,*,#6635,.F.);
#9018=ORIENTED_EDGE('',*,*,#6544,.T.);
#9019=ORIENTED_EDGE('',*,*,#6636,.F.);
#9020=ORIENTED_EDGE('',*,*,#6637,.F.);
#9021=ORIENTED_EDGE('',*,*,#6634,.T.);
#9022=ORIENTED_EDGE('',*,*,#6543,.T.);
#9023=ORIENTED_EDGE('',*,*,#6449,.F.);
#9024=ORIENTED_EDGE('',*,*,#6638,.F.);
#9025=ORIENTED_EDGE('',*,*,#6636,.T.);
#9026=ORIENTED_EDGE('',*,*,#6632,.F.);
#9027=ORIENTED_EDGE('',*,*,#6639,.T.);
#9028=ORIENTED_EDGE('',*,*,#6496,.F.);
#9029=ORIENTED_EDGE('',*,*,#6640,.F.);
#9030=ORIENTED_EDGE('',*,*,#6443,.T.);
#9031=ORIENTED_EDGE('',*,*,#6547,.T.);
#9032=ORIENTED_EDGE('',*,*,#6641,.F.);
#9033=ORIENTED_EDGE('',*,*,#6642,.T.);
#9034=ORIENTED_EDGE('',*,*,#6643,.T.);
#9035=ORIENTED_EDGE('',*,*,#6551,.T.);
#9036=ORIENTED_EDGE('',*,*,#6501,.F.);
#9037=ORIENTED_EDGE('',*,*,#6644,.T.);
#9038=ORIENTED_EDGE('',*,*,#6641,.T.);
#9039=ORIENTED_EDGE('',*,*,#6550,.T.);
#9040=ORIENTED_EDGE('',*,*,#6645,.F.);
#9041=ORIENTED_EDGE('',*,*,#6646,.F.);
#9042=ORIENTED_EDGE('',*,*,#6549,.T.);
#9043=ORIENTED_EDGE('',*,*,#6647,.F.);
#9044=ORIENTED_EDGE('',*,*,#6648,.F.);
#9045=ORIENTED_EDGE('',*,*,#6645,.T.);
#9046=ORIENTED_EDGE('',*,*,#6548,.T.);
#9047=ORIENTED_EDGE('',*,*,#6445,.F.);
#9048=ORIENTED_EDGE('',*,*,#6649,.F.);
#9049=ORIENTED_EDGE('',*,*,#6647,.T.);
#9050=ORIENTED_EDGE('',*,*,#6643,.F.);
#9051=ORIENTED_EDGE('',*,*,#6650,.T.);
#9052=ORIENTED_EDGE('',*,*,#6499,.F.);
#9053=ORIENTED_EDGE('',*,*,#6651,.F.);
#9054=ORIENTED_EDGE('',*,*,#6432,.T.);
#9055=ORIENTED_EDGE('',*,*,#6552,.T.);
#9056=ORIENTED_EDGE('',*,*,#6652,.F.);
#9057=ORIENTED_EDGE('',*,*,#6653,.T.);
#9058=ORIENTED_EDGE('',*,*,#6654,.T.);
#9059=ORIENTED_EDGE('',*,*,#6556,.T.);
#9060=ORIENTED_EDGE('',*,*,#6504,.F.);
#9061=ORIENTED_EDGE('',*,*,#6655,.T.);
#9062=ORIENTED_EDGE('',*,*,#6652,.T.);
#9063=ORIENTED_EDGE('',*,*,#6555,.T.);
#9064=ORIENTED_EDGE('',*,*,#6656,.F.);
#9065=ORIENTED_EDGE('',*,*,#6657,.F.);
#9066=ORIENTED_EDGE('',*,*,#6554,.T.);
#9067=ORIENTED_EDGE('',*,*,#6658,.F.);
#9068=ORIENTED_EDGE('',*,*,#6659,.F.);
#9069=ORIENTED_EDGE('',*,*,#6656,.T.);
#9070=ORIENTED_EDGE('',*,*,#6553,.T.);
#9071=ORIENTED_EDGE('',*,*,#6437,.F.);
#9072=ORIENTED_EDGE('',*,*,#6660,.F.);
#9073=ORIENTED_EDGE('',*,*,#6658,.T.);
#9074=ORIENTED_EDGE('',*,*,#6654,.F.);
#9075=ORIENTED_EDGE('',*,*,#6661,.T.);
#9076=ORIENTED_EDGE('',*,*,#6502,.F.);
#9077=ORIENTED_EDGE('',*,*,#6662,.F.);
#9078=ORIENTED_EDGE('',*,*,#6463,.T.);
#9079=ORIENTED_EDGE('',*,*,#6557,.T.);
#9080=ORIENTED_EDGE('',*,*,#6663,.F.);
#9081=ORIENTED_EDGE('',*,*,#6664,.T.);
#9082=ORIENTED_EDGE('',*,*,#6665,.T.);
#9083=ORIENTED_EDGE('',*,*,#6511,.T.);
#9084=ORIENTED_EDGE('',*,*,#6507,.F.);
#9085=ORIENTED_EDGE('',*,*,#6666,.T.);
#9086=ORIENTED_EDGE('',*,*,#6663,.T.);
#9087=ORIENTED_EDGE('',*,*,#6510,.T.);
#9088=ORIENTED_EDGE('',*,*,#6667,.F.);
#9089=ORIENTED_EDGE('',*,*,#6668,.F.);
#9090=ORIENTED_EDGE('',*,*,#6509,.T.);
#9091=ORIENTED_EDGE('',*,*,#6669,.F.);
#9092=ORIENTED_EDGE('',*,*,#6670,.F.);
#9093=ORIENTED_EDGE('',*,*,#6667,.T.);
#9094=ORIENTED_EDGE('',*,*,#6508,.T.);
#9095=ORIENTED_EDGE('',*,*,#6465,.F.);
#9096=ORIENTED_EDGE('',*,*,#6671,.F.);
#9097=ORIENTED_EDGE('',*,*,#6669,.T.);
#9098=ORIENTED_EDGE('',*,*,#6665,.F.);
#9099=ORIENTED_EDGE('',*,*,#6672,.T.);
#9100=ORIENTED_EDGE('',*,*,#6505,.F.);
#9101=ORIENTED_EDGE('',*,*,#6673,.F.);
#9102=ORIENTED_EDGE('',*,*,#6462,.T.);
#9103=ORIENTED_EDGE('',*,*,#6512,.T.);
#9104=ORIENTED_EDGE('',*,*,#6584,.F.);
#9105=ORIENTED_EDGE('',*,*,#6576,.F.);
#9106=ORIENTED_EDGE('',*,*,#6578,.F.);
#9107=ORIENTED_EDGE('',*,*,#6482,.F.);
#9108=ORIENTED_EDGE('',*,*,#6595,.F.);
#9109=ORIENTED_EDGE('',*,*,#6587,.F.);
#9110=ORIENTED_EDGE('',*,*,#6589,.F.);
#9111=ORIENTED_EDGE('',*,*,#6485,.F.);
#9112=ORIENTED_EDGE('',*,*,#6606,.F.);
#9113=ORIENTED_EDGE('',*,*,#6598,.F.);
#9114=ORIENTED_EDGE('',*,*,#6600,.F.);
#9115=ORIENTED_EDGE('',*,*,#6488,.F.);
#9116=ORIENTED_EDGE('',*,*,#6617,.F.);
#9117=ORIENTED_EDGE('',*,*,#6609,.F.);
#9118=ORIENTED_EDGE('',*,*,#6611,.F.);
#9119=ORIENTED_EDGE('',*,*,#6491,.F.);
#9120=ORIENTED_EDGE('',*,*,#6628,.F.);
#9121=ORIENTED_EDGE('',*,*,#6620,.F.);
#9122=ORIENTED_EDGE('',*,*,#6622,.F.);
#9123=ORIENTED_EDGE('',*,*,#6494,.F.);
#9124=ORIENTED_EDGE('',*,*,#6639,.F.);
#9125=ORIENTED_EDGE('',*,*,#6631,.F.);
#9126=ORIENTED_EDGE('',*,*,#6633,.F.);
#9127=ORIENTED_EDGE('',*,*,#6497,.F.);
#9128=ORIENTED_EDGE('',*,*,#6650,.F.);
#9129=ORIENTED_EDGE('',*,*,#6642,.F.);
#9130=ORIENTED_EDGE('',*,*,#6644,.F.);
#9131=ORIENTED_EDGE('',*,*,#6500,.F.);
#9132=ORIENTED_EDGE('',*,*,#6661,.F.);
#9133=ORIENTED_EDGE('',*,*,#6653,.F.);
#9134=ORIENTED_EDGE('',*,*,#6655,.F.);
#9135=ORIENTED_EDGE('',*,*,#6503,.F.);
#9136=ORIENTED_EDGE('',*,*,#6672,.F.);
#9137=ORIENTED_EDGE('',*,*,#6664,.F.);
#9138=ORIENTED_EDGE('',*,*,#6666,.F.);
#9139=ORIENTED_EDGE('',*,*,#6506,.F.);
#9140=ORIENTED_EDGE('',*,*,#6424,.T.);
#9141=ORIENTED_EDGE('',*,*,#6569,.T.);
#9142=ORIENTED_EDGE('',*,*,#6571,.T.);
#9143=ORIENTED_EDGE('',*,*,#6572,.T.);
#9144=ORIENTED_EDGE('',*,*,#6459,.F.);
#9145=ORIENTED_EDGE('',*,*,#6673,.T.);
#9146=ORIENTED_EDGE('',*,*,#6472,.F.);
#9147=ORIENTED_EDGE('',*,*,#6574,.T.);
#9148=ORIENTED_EDGE('',*,*,#6422,.T.);
#9149=ORIENTED_EDGE('',*,*,#6580,.T.);
#9150=ORIENTED_EDGE('',*,*,#6582,.T.);
#9151=ORIENTED_EDGE('',*,*,#6583,.T.);
#9152=ORIENTED_EDGE('',*,*,#6468,.F.);
#9153=ORIENTED_EDGE('',*,*,#6585,.T.);
#9154=ORIENTED_EDGE('',*,*,#6420,.T.);
#9155=ORIENTED_EDGE('',*,*,#6591,.T.);
#9156=ORIENTED_EDGE('',*,*,#6593,.T.);
#9157=ORIENTED_EDGE('',*,*,#6594,.T.);
#9158=ORIENTED_EDGE('',*,*,#6439,.F.);
#9159=ORIENTED_EDGE('',*,*,#6596,.T.);
#9160=ORIENTED_EDGE('',*,*,#6418,.T.);
#9161=ORIENTED_EDGE('',*,*,#6602,.T.);
#9162=ORIENTED_EDGE('',*,*,#6604,.T.);
#9163=ORIENTED_EDGE('',*,*,#6605,.T.);
#9164=ORIENTED_EDGE('',*,*,#6456,.F.);
#9165=ORIENTED_EDGE('',*,*,#6607,.T.);
#9166=ORIENTED_EDGE('',*,*,#6416,.T.);
#9167=ORIENTED_EDGE('',*,*,#6613,.T.);
#9168=ORIENTED_EDGE('',*,*,#6615,.T.);
#9169=ORIENTED_EDGE('',*,*,#6616,.T.);
#9170=ORIENTED_EDGE('',*,*,#6452,.F.);
#9171=ORIENTED_EDGE('',*,*,#6618,.T.);
#9172=ORIENTED_EDGE('',*,*,#6414,.T.);
#9173=ORIENTED_EDGE('',*,*,#6624,.T.);
#9174=ORIENTED_EDGE('',*,*,#6626,.T.);
#9175=ORIENTED_EDGE('',*,*,#6627,.T.);
#9176=ORIENTED_EDGE('',*,*,#6448,.F.);
#9177=ORIENTED_EDGE('',*,*,#6629,.T.);
#9178=ORIENTED_EDGE('',*,*,#6412,.T.);
#9179=ORIENTED_EDGE('',*,*,#6635,.T.);
#9180=ORIENTED_EDGE('',*,*,#6637,.T.);
#9181=ORIENTED_EDGE('',*,*,#6638,.T.);
#9182=ORIENTED_EDGE('',*,*,#6444,.F.);
#9183=ORIENTED_EDGE('',*,*,#6640,.T.);
#9184=ORIENTED_EDGE('',*,*,#6410,.T.);
#9185=ORIENTED_EDGE('',*,*,#6646,.T.);
#9186=ORIENTED_EDGE('',*,*,#6648,.T.);
#9187=ORIENTED_EDGE('',*,*,#6649,.T.);
#9188=ORIENTED_EDGE('',*,*,#6433,.F.);
#9189=ORIENTED_EDGE('',*,*,#6651,.T.);
#9190=ORIENTED_EDGE('',*,*,#6408,.T.);
#9191=ORIENTED_EDGE('',*,*,#6428,.T.);
#9192=ORIENTED_EDGE('',*,*,#6657,.T.);
#9193=ORIENTED_EDGE('',*,*,#6659,.T.);
#9194=ORIENTED_EDGE('',*,*,#6660,.T.);
#9195=ORIENTED_EDGE('',*,*,#6436,.F.);
#9196=ORIENTED_EDGE('',*,*,#6464,.F.);
#9197=ORIENTED_EDGE('',*,*,#6662,.T.);
#9198=ORIENTED_EDGE('',*,*,#6426,.T.);
#9199=ORIENTED_EDGE('',*,*,#6668,.T.);
#9200=ORIENTED_EDGE('',*,*,#6670,.T.);
#9201=ORIENTED_EDGE('',*,*,#6671,.T.);
#9202=ORIENTED_EDGE('',*,*,#6435,.T.);
#9203=ORIENTED_EDGE('',*,*,#6406,.F.);
#9204=ORIENTED_EDGE('',*,*,#6558,.T.);
#9205=ORIENTED_EDGE('',*,*,#6674,.T.);
#9206=ORIENTED_EDGE('',*,*,#6561,.T.);
#9207=ORIENTED_EDGE('',*,*,#6403,.F.);
#9208=ORIENTED_EDGE('',*,*,#6560,.T.);
#9209=ORIENTED_EDGE('',*,*,#6675,.T.);
#9210=ORIENTED_EDGE('',*,*,#6562,.T.);
#9211=ORIENTED_EDGE('',*,*,#6674,.F.);
#9212=ORIENTED_EDGE('',*,*,#6559,.T.);
#9213=ORIENTED_EDGE('',*,*,#6405,.T.);
#9214=ORIENTED_EDGE('',*,*,#6563,.T.);
#9215=ORIENTED_EDGE('',*,*,#6675,.F.);
#9216=ORIENTED_EDGE('',*,*,#6676,.F.);
#9217=ORIENTED_EDGE('',*,*,#6677,.T.);
#9218=ORIENTED_EDGE('',*,*,#6678,.F.);
#9219=ORIENTED_EDGE('',*,*,#6679,.F.);
#9220=ORIENTED_EDGE('',*,*,#6677,.F.);
#9221=ORIENTED_EDGE('',*,*,#6680,.F.);
#9222=ORIENTED_EDGE('',*,*,#6681,.F.);
#9223=ORIENTED_EDGE('',*,*,#6682,.T.);
#9224=ORIENTED_EDGE('',*,*,#6683,.F.);
#9225=ORIENTED_EDGE('',*,*,#6682,.F.);
#9226=ORIENTED_EDGE('',*,*,#6684,.F.);
#9227=ORIENTED_EDGE('',*,*,#6685,.T.);
#9228=ORIENTED_EDGE('',*,*,#6686,.T.);
#9229=ORIENTED_EDGE('',*,*,#6685,.F.);
#9230=ORIENTED_EDGE('',*,*,#6687,.F.);
#9231=ORIENTED_EDGE('',*,*,#6688,.T.);
#9232=ORIENTED_EDGE('',*,*,#6684,.T.);
#9233=ORIENTED_EDGE('',*,*,#6688,.F.);
#9234=ORIENTED_EDGE('',*,*,#6689,.F.);
#9235=ORIENTED_EDGE('',*,*,#6690,.T.);
#9236=ORIENTED_EDGE('',*,*,#6691,.T.);
#9237=ORIENTED_EDGE('',*,*,#6690,.F.);
#9238=ORIENTED_EDGE('',*,*,#6692,.F.);
#9239=ORIENTED_EDGE('',*,*,#6693,.T.);
#9240=ORIENTED_EDGE('',*,*,#6689,.T.);
#9241=ORIENTED_EDGE('',*,*,#6693,.F.);
#9242=ORIENTED_EDGE('',*,*,#6694,.F.);
#9243=ORIENTED_EDGE('',*,*,#6695,.T.);
#9244=ORIENTED_EDGE('',*,*,#6696,.T.);
#9245=ORIENTED_EDGE('',*,*,#6695,.F.);
#9246=ORIENTED_EDGE('',*,*,#6697,.F.);
#9247=ORIENTED_EDGE('',*,*,#6698,.T.);
#9248=ORIENTED_EDGE('',*,*,#6694,.T.);
#9249=ORIENTED_EDGE('',*,*,#6698,.F.);
#9250=ORIENTED_EDGE('',*,*,#6699,.F.);
#9251=ORIENTED_EDGE('',*,*,#6700,.T.);
#9252=ORIENTED_EDGE('',*,*,#6701,.T.);
#9253=ORIENTED_EDGE('',*,*,#6700,.F.);
#9254=ORIENTED_EDGE('',*,*,#6702,.F.);
#9255=ORIENTED_EDGE('',*,*,#6703,.T.);
#9256=ORIENTED_EDGE('',*,*,#6699,.T.);
#9257=ORIENTED_EDGE('',*,*,#6703,.F.);
#9258=ORIENTED_EDGE('',*,*,#6704,.F.);
#9259=ORIENTED_EDGE('',*,*,#6705,.T.);
#9260=ORIENTED_EDGE('',*,*,#6706,.T.);
#9261=ORIENTED_EDGE('',*,*,#6705,.F.);
#9262=ORIENTED_EDGE('',*,*,#6707,.F.);
#9263=ORIENTED_EDGE('',*,*,#6708,.T.);
#9264=ORIENTED_EDGE('',*,*,#6704,.T.);
#9265=ORIENTED_EDGE('',*,*,#6708,.F.);
#9266=ORIENTED_EDGE('',*,*,#6709,.F.);
#9267=ORIENTED_EDGE('',*,*,#6710,.T.);
#9268=ORIENTED_EDGE('',*,*,#6711,.T.);
#9269=ORIENTED_EDGE('',*,*,#6710,.F.);
#9270=ORIENTED_EDGE('',*,*,#6712,.F.);
#9271=ORIENTED_EDGE('',*,*,#6713,.T.);
#9272=ORIENTED_EDGE('',*,*,#6709,.T.);
#9273=ORIENTED_EDGE('',*,*,#6713,.F.);
#9274=ORIENTED_EDGE('',*,*,#6714,.T.);
#9275=ORIENTED_EDGE('',*,*,#6715,.T.);
#9276=ORIENTED_EDGE('',*,*,#6716,.F.);
#9277=ORIENTED_EDGE('',*,*,#6715,.F.);
#9278=ORIENTED_EDGE('',*,*,#6680,.T.);
#9279=ORIENTED_EDGE('',*,*,#6681,.T.);
#9280=ORIENTED_EDGE('',*,*,#6717,.T.);
#9281=ORIENTED_EDGE('',*,*,#6678,.T.);
#9282=ORIENTED_EDGE('',*,*,#6679,.T.);
#9283=ORIENTED_EDGE('',*,*,#6717,.F.);
#9284=ORIENTED_EDGE('',*,*,#6676,.T.);
#9285=ORIENTED_EDGE('',*,*,#6686,.F.);
#9286=ORIENTED_EDGE('',*,*,#6691,.F.);
#9287=ORIENTED_EDGE('',*,*,#6696,.F.);
#9288=ORIENTED_EDGE('',*,*,#6701,.F.);
#9289=ORIENTED_EDGE('',*,*,#6706,.F.);
#9290=ORIENTED_EDGE('',*,*,#6711,.F.);
#9291=ORIENTED_EDGE('',*,*,#6714,.F.);
#9292=ORIENTED_EDGE('',*,*,#6683,.T.);
#9293=ORIENTED_EDGE('',*,*,#6687,.T.);
#9294=ORIENTED_EDGE('',*,*,#6692,.T.);
#9295=ORIENTED_EDGE('',*,*,#6697,.T.);
#9296=ORIENTED_EDGE('',*,*,#6702,.T.);
#9297=ORIENTED_EDGE('',*,*,#6707,.T.);
#9298=ORIENTED_EDGE('',*,*,#6712,.T.);
#9299=ORIENTED_EDGE('',*,*,#6716,.T.);
#9300=ORIENTED_EDGE('',*,*,#6718,.F.);
#9301=ORIENTED_EDGE('',*,*,#6719,.F.);
#9302=ORIENTED_EDGE('',*,*,#6720,.F.);
#9303=ORIENTED_EDGE('',*,*,#6721,.T.);
#9304=ORIENTED_EDGE('',*,*,#6722,.F.);
#9305=ORIENTED_EDGE('',*,*,#6723,.F.);
#9306=ORIENTED_EDGE('',*,*,#6724,.F.);
#9307=ORIENTED_EDGE('',*,*,#6719,.T.);
#9308=ORIENTED_EDGE('',*,*,#6725,.F.);
#9309=ORIENTED_EDGE('',*,*,#6726,.F.);
#9310=ORIENTED_EDGE('',*,*,#6727,.F.);
#9311=ORIENTED_EDGE('',*,*,#6723,.T.);
#9312=ORIENTED_EDGE('',*,*,#6728,.F.);
#9313=ORIENTED_EDGE('',*,*,#6729,.F.);
#9314=ORIENTED_EDGE('',*,*,#6730,.F.);
#9315=ORIENTED_EDGE('',*,*,#6726,.T.);
#9316=ORIENTED_EDGE('',*,*,#6731,.F.);
#9317=ORIENTED_EDGE('',*,*,#6732,.F.);
#9318=ORIENTED_EDGE('',*,*,#6733,.F.);
#9319=ORIENTED_EDGE('',*,*,#6729,.T.);
#9320=ORIENTED_EDGE('',*,*,#6734,.F.);
#9321=ORIENTED_EDGE('',*,*,#6735,.F.);
#9322=ORIENTED_EDGE('',*,*,#6736,.F.);
#9323=ORIENTED_EDGE('',*,*,#6732,.T.);
#9324=ORIENTED_EDGE('',*,*,#6737,.F.);
#9325=ORIENTED_EDGE('',*,*,#6738,.F.);
#9326=ORIENTED_EDGE('',*,*,#6739,.F.);
#9327=ORIENTED_EDGE('',*,*,#6735,.T.);
#9328=ORIENTED_EDGE('',*,*,#6740,.F.);
#9329=ORIENTED_EDGE('',*,*,#6741,.F.);
#9330=ORIENTED_EDGE('',*,*,#6742,.F.);
#9331=ORIENTED_EDGE('',*,*,#6738,.T.);
#9332=ORIENTED_EDGE('',*,*,#6743,.F.);
#9333=ORIENTED_EDGE('',*,*,#6744,.F.);
#9334=ORIENTED_EDGE('',*,*,#6745,.F.);
#9335=ORIENTED_EDGE('',*,*,#6741,.T.);
#9336=ORIENTED_EDGE('',*,*,#6746,.F.);
#9337=ORIENTED_EDGE('',*,*,#6747,.F.);
#9338=ORIENTED_EDGE('',*,*,#6748,.F.);
#9339=ORIENTED_EDGE('',*,*,#6744,.T.);
#9340=ORIENTED_EDGE('',*,*,#6749,.F.);
#9341=ORIENTED_EDGE('',*,*,#6750,.F.);
#9342=ORIENTED_EDGE('',*,*,#6751,.F.);
#9343=ORIENTED_EDGE('',*,*,#6747,.T.);
#9344=ORIENTED_EDGE('',*,*,#6752,.F.);
#9345=ORIENTED_EDGE('',*,*,#6721,.F.);
#9346=ORIENTED_EDGE('',*,*,#6753,.F.);
#9347=ORIENTED_EDGE('',*,*,#6750,.T.);
#9348=ORIENTED_EDGE('',*,*,#6753,.T.);
#9349=ORIENTED_EDGE('',*,*,#6720,.T.);
#9350=ORIENTED_EDGE('',*,*,#6724,.T.);
#9351=ORIENTED_EDGE('',*,*,#6727,.T.);
#9352=ORIENTED_EDGE('',*,*,#6730,.T.);
#9353=ORIENTED_EDGE('',*,*,#6733,.T.);
#9354=ORIENTED_EDGE('',*,*,#6736,.T.);
#9355=ORIENTED_EDGE('',*,*,#6739,.T.);
#9356=ORIENTED_EDGE('',*,*,#6742,.T.);
#9357=ORIENTED_EDGE('',*,*,#6745,.T.);
#9358=ORIENTED_EDGE('',*,*,#6748,.T.);
#9359=ORIENTED_EDGE('',*,*,#6751,.T.);
#9360=ORIENTED_EDGE('',*,*,#6722,.T.);
#9361=ORIENTED_EDGE('',*,*,#6718,.T.);
#9362=ORIENTED_EDGE('',*,*,#6752,.T.);
#9363=ORIENTED_EDGE('',*,*,#6749,.T.);
#9364=ORIENTED_EDGE('',*,*,#6746,.T.);
#9365=ORIENTED_EDGE('',*,*,#6743,.T.);
#9366=ORIENTED_EDGE('',*,*,#6740,.T.);
#9367=ORIENTED_EDGE('',*,*,#6737,.T.);
#9368=ORIENTED_EDGE('',*,*,#6734,.T.);
#9369=ORIENTED_EDGE('',*,*,#6731,.T.);
#9370=ORIENTED_EDGE('',*,*,#6728,.T.);
#9371=ORIENTED_EDGE('',*,*,#6725,.T.);
#9372=ORIENTED_EDGE('',*,*,#6754,.T.);
#9373=ORIENTED_EDGE('',*,*,#6755,.T.);
#9374=ORIENTED_EDGE('',*,*,#6756,.T.);
#9375=ORIENTED_EDGE('',*,*,#6757,.T.);
#9376=ORIENTED_EDGE('',*,*,#6758,.T.);
#9377=ORIENTED_EDGE('',*,*,#6759,.T.);
#9378=ORIENTED_EDGE('',*,*,#6760,.T.);
#9379=ORIENTED_EDGE('',*,*,#6761,.T.);
#9380=ORIENTED_EDGE('',*,*,#6762,.T.);
#9381=ORIENTED_EDGE('',*,*,#6763,.F.);
#9382=ORIENTED_EDGE('',*,*,#6764,.T.);
#9383=ORIENTED_EDGE('',*,*,#6765,.T.);
#9384=ORIENTED_EDGE('',*,*,#6766,.T.);
#9385=ORIENTED_EDGE('',*,*,#6767,.T.);
#9386=ORIENTED_EDGE('',*,*,#6768,.F.);
#9387=ORIENTED_EDGE('',*,*,#6764,.F.);
#9388=ORIENTED_EDGE('',*,*,#6769,.T.);
#9389=ORIENTED_EDGE('',*,*,#6770,.T.);
#9390=ORIENTED_EDGE('',*,*,#6766,.F.);
#9391=ORIENTED_EDGE('',*,*,#6763,.T.);
#9392=ORIENTED_EDGE('',*,*,#6771,.T.);
#9393=ORIENTED_EDGE('',*,*,#6772,.T.);
#9394=ORIENTED_EDGE('',*,*,#6769,.F.);
#9395=ORIENTED_EDGE('',*,*,#6762,.F.);
#9396=ORIENTED_EDGE('',*,*,#6773,.T.);
#9397=ORIENTED_EDGE('',*,*,#6774,.T.);
#9398=ORIENTED_EDGE('',*,*,#6771,.F.);
#9399=ORIENTED_EDGE('',*,*,#6761,.F.);
#9400=ORIENTED_EDGE('',*,*,#6775,.T.);
#9401=ORIENTED_EDGE('',*,*,#6776,.T.);
#9402=ORIENTED_EDGE('',*,*,#6773,.F.);
#9403=ORIENTED_EDGE('',*,*,#6760,.F.);
#9404=ORIENTED_EDGE('',*,*,#6777,.T.);
#9405=ORIENTED_EDGE('',*,*,#6778,.T.);
#9406=ORIENTED_EDGE('',*,*,#6775,.F.);
#9407=ORIENTED_EDGE('',*,*,#6759,.F.);
#9408=ORIENTED_EDGE('',*,*,#6779,.T.);
#9409=ORIENTED_EDGE('',*,*,#6780,.T.);
#9410=ORIENTED_EDGE('',*,*,#6777,.F.);
#9411=ORIENTED_EDGE('',*,*,#6758,.F.);
#9412=ORIENTED_EDGE('',*,*,#6781,.T.);
#9413=ORIENTED_EDGE('',*,*,#6782,.T.);
#9414=ORIENTED_EDGE('',*,*,#6779,.F.);
#9415=ORIENTED_EDGE('',*,*,#6757,.F.);
#9416=ORIENTED_EDGE('',*,*,#6783,.T.);
#9417=ORIENTED_EDGE('',*,*,#6784,.T.);
#9418=ORIENTED_EDGE('',*,*,#6781,.F.);
#9419=ORIENTED_EDGE('',*,*,#6756,.F.);
#9420=ORIENTED_EDGE('',*,*,#6785,.T.);
#9421=ORIENTED_EDGE('',*,*,#6786,.T.);
#9422=ORIENTED_EDGE('',*,*,#6783,.F.);
#9423=ORIENTED_EDGE('',*,*,#6755,.F.);
#9424=ORIENTED_EDGE('',*,*,#6787,.T.);
#9425=ORIENTED_EDGE('',*,*,#6788,.T.);
#9426=ORIENTED_EDGE('',*,*,#6785,.F.);
#9427=ORIENTED_EDGE('',*,*,#6754,.F.);
#9428=ORIENTED_EDGE('',*,*,#6768,.T.);
#9429=ORIENTED_EDGE('',*,*,#6789,.T.);
#9430=ORIENTED_EDGE('',*,*,#6787,.F.);
#9431=ORIENTED_EDGE('',*,*,#6765,.F.);
#9432=ORIENTED_EDGE('',*,*,#6767,.F.);
#9433=ORIENTED_EDGE('',*,*,#6770,.F.);
#9434=ORIENTED_EDGE('',*,*,#6772,.F.);
#9435=ORIENTED_EDGE('',*,*,#6774,.F.);
#9436=ORIENTED_EDGE('',*,*,#6776,.F.);
#9437=ORIENTED_EDGE('',*,*,#6778,.F.);
#9438=ORIENTED_EDGE('',*,*,#6780,.F.);
#9439=ORIENTED_EDGE('',*,*,#6782,.F.);
#9440=ORIENTED_EDGE('',*,*,#6784,.F.);
#9441=ORIENTED_EDGE('',*,*,#6786,.F.);
#9442=ORIENTED_EDGE('',*,*,#6788,.F.);
#9443=ORIENTED_EDGE('',*,*,#6789,.F.);
#9444=ORIENTED_EDGE('',*,*,#6790,.T.);
#9445=ORIENTED_EDGE('',*,*,#6791,.T.);
#9446=ORIENTED_EDGE('',*,*,#6792,.T.);
#9447=ORIENTED_EDGE('',*,*,#6793,.T.);
#9448=ORIENTED_EDGE('',*,*,#6794,.T.);
#9449=ORIENTED_EDGE('',*,*,#6795,.T.);
#9450=ORIENTED_EDGE('',*,*,#6796,.T.);
#9451=ORIENTED_EDGE('',*,*,#6797,.T.);
#9452=ORIENTED_EDGE('',*,*,#6798,.T.);
#9453=ORIENTED_EDGE('',*,*,#6799,.T.);
#9454=ORIENTED_EDGE('',*,*,#6800,.T.);
#9455=ORIENTED_EDGE('',*,*,#6801,.T.);
#9456=ORIENTED_EDGE('',*,*,#6802,.F.);
#9457=ORIENTED_EDGE('',*,*,#6803,.T.);
#9458=ORIENTED_EDGE('',*,*,#6804,.T.);
#9459=ORIENTED_EDGE('',*,*,#6792,.F.);
#9460=ORIENTED_EDGE('',*,*,#6804,.F.);
#9461=ORIENTED_EDGE('',*,*,#6805,.T.);
#9462=ORIENTED_EDGE('',*,*,#6806,.T.);
#9463=ORIENTED_EDGE('',*,*,#6793,.F.);
#9464=ORIENTED_EDGE('',*,*,#6806,.F.);
#9465=ORIENTED_EDGE('',*,*,#6807,.T.);
#9466=ORIENTED_EDGE('',*,*,#6808,.T.);
#9467=ORIENTED_EDGE('',*,*,#6794,.F.);
#9468=ORIENTED_EDGE('',*,*,#6808,.F.);
#9469=ORIENTED_EDGE('',*,*,#6809,.T.);
#9470=ORIENTED_EDGE('',*,*,#6810,.T.);
#9471=ORIENTED_EDGE('',*,*,#6795,.F.);
#9472=ORIENTED_EDGE('',*,*,#6810,.F.);
#9473=ORIENTED_EDGE('',*,*,#6811,.T.);
#9474=ORIENTED_EDGE('',*,*,#6812,.T.);
#9475=ORIENTED_EDGE('',*,*,#6796,.F.);
#9476=ORIENTED_EDGE('',*,*,#6812,.F.);
#9477=ORIENTED_EDGE('',*,*,#6813,.T.);
#9478=ORIENTED_EDGE('',*,*,#6814,.T.);
#9479=ORIENTED_EDGE('',*,*,#6797,.F.);
#9480=ORIENTED_EDGE('',*,*,#6814,.F.);
#9481=ORIENTED_EDGE('',*,*,#6815,.T.);
#9482=ORIENTED_EDGE('',*,*,#6816,.T.);
#9483=ORIENTED_EDGE('',*,*,#6798,.F.);
#9484=ORIENTED_EDGE('',*,*,#6816,.F.);
#9485=ORIENTED_EDGE('',*,*,#6817,.T.);
#9486=ORIENTED_EDGE('',*,*,#6818,.T.);
#9487=ORIENTED_EDGE('',*,*,#6799,.F.);
#9488=ORIENTED_EDGE('',*,*,#6818,.F.);
#9489=ORIENTED_EDGE('',*,*,#6819,.T.);
#9490=ORIENTED_EDGE('',*,*,#6820,.T.);
#9491=ORIENTED_EDGE('',*,*,#6800,.F.);
#9492=ORIENTED_EDGE('',*,*,#6820,.F.);
#9493=ORIENTED_EDGE('',*,*,#6821,.T.);
#9494=ORIENTED_EDGE('',*,*,#6822,.T.);
#9495=ORIENTED_EDGE('',*,*,#6801,.F.);
#9496=ORIENTED_EDGE('',*,*,#6822,.F.);
#9497=ORIENTED_EDGE('',*,*,#6823,.T.);
#9498=ORIENTED_EDGE('',*,*,#6824,.T.);
#9499=ORIENTED_EDGE('',*,*,#6790,.F.);
#9500=ORIENTED_EDGE('',*,*,#6824,.F.);
#9501=ORIENTED_EDGE('',*,*,#6825,.T.);
#9502=ORIENTED_EDGE('',*,*,#6802,.T.);
#9503=ORIENTED_EDGE('',*,*,#6791,.F.);
#9504=ORIENTED_EDGE('',*,*,#6823,.F.);
#9505=ORIENTED_EDGE('',*,*,#6821,.F.);
#9506=ORIENTED_EDGE('',*,*,#6819,.F.);
#9507=ORIENTED_EDGE('',*,*,#6817,.F.);
#9508=ORIENTED_EDGE('',*,*,#6815,.F.);
#9509=ORIENTED_EDGE('',*,*,#6813,.F.);
#9510=ORIENTED_EDGE('',*,*,#6811,.F.);
#9511=ORIENTED_EDGE('',*,*,#6809,.F.);
#9512=ORIENTED_EDGE('',*,*,#6807,.F.);
#9513=ORIENTED_EDGE('',*,*,#6805,.F.);
#9514=ORIENTED_EDGE('',*,*,#6803,.F.);
#9515=ORIENTED_EDGE('',*,*,#6825,.F.);
#9516=ORIENTED_EDGE('',*,*,#6826,.T.);
#9517=ORIENTED_EDGE('',*,*,#6827,.T.);
#9518=ORIENTED_EDGE('',*,*,#6828,.F.);
#9519=ORIENTED_EDGE('',*,*,#6829,.F.);
#9520=ORIENTED_EDGE('',*,*,#6830,.F.);
#9521=ORIENTED_EDGE('',*,*,#6829,.T.);
#9522=ORIENTED_EDGE('',*,*,#6831,.F.);
#9523=ORIENTED_EDGE('',*,*,#6832,.F.);
#9524=ORIENTED_EDGE('',*,*,#6833,.F.);
#9525=ORIENTED_EDGE('',*,*,#6832,.T.);
#9526=ORIENTED_EDGE('',*,*,#6834,.F.);
#9527=ORIENTED_EDGE('',*,*,#6835,.F.);
#9528=ORIENTED_EDGE('',*,*,#6836,.F.);
#9529=ORIENTED_EDGE('',*,*,#6835,.T.);
#9530=ORIENTED_EDGE('',*,*,#6837,.F.);
#9531=ORIENTED_EDGE('',*,*,#6838,.F.);
#9532=ORIENTED_EDGE('',*,*,#6839,.F.);
#9533=ORIENTED_EDGE('',*,*,#6838,.T.);
#9534=ORIENTED_EDGE('',*,*,#6840,.F.);
#9535=ORIENTED_EDGE('',*,*,#6841,.F.);
#9536=ORIENTED_EDGE('',*,*,#6842,.F.);
#9537=ORIENTED_EDGE('',*,*,#6841,.T.);
#9538=ORIENTED_EDGE('',*,*,#6843,.F.);
#9539=ORIENTED_EDGE('',*,*,#6844,.F.);
#9540=ORIENTED_EDGE('',*,*,#6845,.F.);
#9541=ORIENTED_EDGE('',*,*,#6844,.T.);
#9542=ORIENTED_EDGE('',*,*,#6846,.F.);
#9543=ORIENTED_EDGE('',*,*,#6847,.F.);
#9544=ORIENTED_EDGE('',*,*,#6848,.F.);
#9545=ORIENTED_EDGE('',*,*,#6847,.T.);
#9546=ORIENTED_EDGE('',*,*,#6849,.F.);
#9547=ORIENTED_EDGE('',*,*,#6850,.F.);
#9548=ORIENTED_EDGE('',*,*,#6851,.F.);
#9549=ORIENTED_EDGE('',*,*,#6850,.T.);
#9550=ORIENTED_EDGE('',*,*,#6852,.F.);
#9551=ORIENTED_EDGE('',*,*,#6853,.F.);
#9552=ORIENTED_EDGE('',*,*,#6854,.F.);
#9553=ORIENTED_EDGE('',*,*,#6853,.T.);
#9554=ORIENTED_EDGE('',*,*,#6855,.F.);
#9555=ORIENTED_EDGE('',*,*,#6856,.F.);
#9556=ORIENTED_EDGE('',*,*,#6857,.F.);
#9557=ORIENTED_EDGE('',*,*,#6856,.T.);
#9558=ORIENTED_EDGE('',*,*,#6858,.F.);
#9559=ORIENTED_EDGE('',*,*,#6859,.F.);
#9560=ORIENTED_EDGE('',*,*,#6860,.F.);
#9561=ORIENTED_EDGE('',*,*,#6859,.T.);
#9562=ORIENTED_EDGE('',*,*,#6861,.F.);
#9563=ORIENTED_EDGE('',*,*,#6827,.F.);
#9564=ORIENTED_EDGE('',*,*,#6831,.T.);
#9565=ORIENTED_EDGE('',*,*,#6828,.T.);
#9566=ORIENTED_EDGE('',*,*,#6861,.T.);
#9567=ORIENTED_EDGE('',*,*,#6858,.T.);
#9568=ORIENTED_EDGE('',*,*,#6855,.T.);
#9569=ORIENTED_EDGE('',*,*,#6852,.T.);
#9570=ORIENTED_EDGE('',*,*,#6849,.T.);
#9571=ORIENTED_EDGE('',*,*,#6846,.T.);
#9572=ORIENTED_EDGE('',*,*,#6843,.T.);
#9573=ORIENTED_EDGE('',*,*,#6840,.T.);
#9574=ORIENTED_EDGE('',*,*,#6837,.T.);
#9575=ORIENTED_EDGE('',*,*,#6834,.T.);
#9576=ORIENTED_EDGE('',*,*,#6830,.T.);
#9577=ORIENTED_EDGE('',*,*,#6833,.T.);
#9578=ORIENTED_EDGE('',*,*,#6836,.T.);
#9579=ORIENTED_EDGE('',*,*,#6839,.T.);
#9580=ORIENTED_EDGE('',*,*,#6842,.T.);
#9581=ORIENTED_EDGE('',*,*,#6845,.T.);
#9582=ORIENTED_EDGE('',*,*,#6848,.T.);
#9583=ORIENTED_EDGE('',*,*,#6851,.T.);
#9584=ORIENTED_EDGE('',*,*,#6854,.T.);
#9585=ORIENTED_EDGE('',*,*,#6857,.T.);
#9586=ORIENTED_EDGE('',*,*,#6860,.T.);
#9587=ORIENTED_EDGE('',*,*,#6826,.F.);
#9588=ORIENTED_EDGE('',*,*,#6862,.F.);
#9589=ORIENTED_EDGE('',*,*,#6863,.F.);
#9590=ORIENTED_EDGE('',*,*,#6864,.F.);
#9591=ORIENTED_EDGE('',*,*,#6865,.T.);
#9592=ORIENTED_EDGE('',*,*,#6866,.F.);
#9593=ORIENTED_EDGE('',*,*,#6867,.F.);
#9594=ORIENTED_EDGE('',*,*,#6868,.F.);
#9595=ORIENTED_EDGE('',*,*,#6863,.T.);
#9596=ORIENTED_EDGE('',*,*,#6869,.F.);
#9597=ORIENTED_EDGE('',*,*,#6870,.F.);
#9598=ORIENTED_EDGE('',*,*,#6871,.F.);
#9599=ORIENTED_EDGE('',*,*,#6867,.T.);
#9600=ORIENTED_EDGE('',*,*,#6872,.F.);
#9601=ORIENTED_EDGE('',*,*,#6873,.F.);
#9602=ORIENTED_EDGE('',*,*,#6874,.F.);
#9603=ORIENTED_EDGE('',*,*,#6870,.T.);
#9604=ORIENTED_EDGE('',*,*,#6875,.F.);
#9605=ORIENTED_EDGE('',*,*,#6876,.F.);
#9606=ORIENTED_EDGE('',*,*,#6877,.F.);
#9607=ORIENTED_EDGE('',*,*,#6873,.T.);
#9608=ORIENTED_EDGE('',*,*,#6878,.F.);
#9609=ORIENTED_EDGE('',*,*,#6879,.F.);
#9610=ORIENTED_EDGE('',*,*,#6880,.F.);
#9611=ORIENTED_EDGE('',*,*,#6876,.T.);
#9612=ORIENTED_EDGE('',*,*,#6881,.F.);
#9613=ORIENTED_EDGE('',*,*,#6882,.F.);
#9614=ORIENTED_EDGE('',*,*,#6883,.F.);
#9615=ORIENTED_EDGE('',*,*,#6879,.T.);
#9616=ORIENTED_EDGE('',*,*,#6884,.F.);
#9617=ORIENTED_EDGE('',*,*,#6885,.F.);
#9618=ORIENTED_EDGE('',*,*,#6886,.F.);
#9619=ORIENTED_EDGE('',*,*,#6882,.T.);
#9620=ORIENTED_EDGE('',*,*,#6887,.F.);
#9621=ORIENTED_EDGE('',*,*,#6888,.F.);
#9622=ORIENTED_EDGE('',*,*,#6889,.F.);
#9623=ORIENTED_EDGE('',*,*,#6885,.T.);
#9624=ORIENTED_EDGE('',*,*,#6890,.F.);
#9625=ORIENTED_EDGE('',*,*,#6891,.F.);
#9626=ORIENTED_EDGE('',*,*,#6892,.F.);
#9627=ORIENTED_EDGE('',*,*,#6888,.T.);
#9628=ORIENTED_EDGE('',*,*,#6893,.F.);
#9629=ORIENTED_EDGE('',*,*,#6894,.F.);
#9630=ORIENTED_EDGE('',*,*,#6895,.F.);
#9631=ORIENTED_EDGE('',*,*,#6891,.T.);
#9632=ORIENTED_EDGE('',*,*,#6896,.F.);
#9633=ORIENTED_EDGE('',*,*,#6865,.F.);
#9634=ORIENTED_EDGE('',*,*,#6897,.F.);
#9635=ORIENTED_EDGE('',*,*,#6894,.T.);
#9636=ORIENTED_EDGE('',*,*,#6897,.T.);
#9637=ORIENTED_EDGE('',*,*,#6864,.T.);
#9638=ORIENTED_EDGE('',*,*,#6868,.T.);
#9639=ORIENTED_EDGE('',*,*,#6871,.T.);
#9640=ORIENTED_EDGE('',*,*,#6874,.T.);
#9641=ORIENTED_EDGE('',*,*,#6877,.T.);
#9642=ORIENTED_EDGE('',*,*,#6880,.T.);
#9643=ORIENTED_EDGE('',*,*,#6883,.T.);
#9644=ORIENTED_EDGE('',*,*,#6886,.T.);
#9645=ORIENTED_EDGE('',*,*,#6889,.T.);
#9646=ORIENTED_EDGE('',*,*,#6892,.T.);
#9647=ORIENTED_EDGE('',*,*,#6895,.T.);
#9648=ORIENTED_EDGE('',*,*,#6866,.T.);
#9649=ORIENTED_EDGE('',*,*,#6862,.T.);
#9650=ORIENTED_EDGE('',*,*,#6896,.T.);
#9651=ORIENTED_EDGE('',*,*,#6893,.T.);
#9652=ORIENTED_EDGE('',*,*,#6890,.T.);
#9653=ORIENTED_EDGE('',*,*,#6887,.T.);
#9654=ORIENTED_EDGE('',*,*,#6884,.T.);
#9655=ORIENTED_EDGE('',*,*,#6881,.T.);
#9656=ORIENTED_EDGE('',*,*,#6878,.T.);
#9657=ORIENTED_EDGE('',*,*,#6875,.T.);
#9658=ORIENTED_EDGE('',*,*,#6872,.T.);
#9659=ORIENTED_EDGE('',*,*,#6869,.T.);
#9660=ORIENTED_EDGE('',*,*,#6898,.T.);
#9661=ORIENTED_EDGE('',*,*,#6899,.T.);
#9662=ORIENTED_EDGE('',*,*,#6900,.T.);
#9663=ORIENTED_EDGE('',*,*,#6901,.F.);
#9664=ORIENTED_EDGE('',*,*,#6902,.T.);
#9665=ORIENTED_EDGE('',*,*,#6903,.T.);
#9666=ORIENTED_EDGE('',*,*,#6904,.T.);
#9667=ORIENTED_EDGE('',*,*,#6905,.T.);
#9668=ORIENTED_EDGE('',*,*,#6906,.T.);
#9669=ORIENTED_EDGE('',*,*,#6907,.T.);
#9670=ORIENTED_EDGE('',*,*,#6908,.T.);
#9671=ORIENTED_EDGE('',*,*,#6909,.T.);
#9672=ORIENTED_EDGE('',*,*,#6910,.F.);
#9673=ORIENTED_EDGE('',*,*,#6911,.T.);
#9674=ORIENTED_EDGE('',*,*,#6912,.T.);
#9675=ORIENTED_EDGE('',*,*,#6900,.F.);
#9676=ORIENTED_EDGE('',*,*,#6912,.F.);
#9677=ORIENTED_EDGE('',*,*,#6913,.T.);
#9678=ORIENTED_EDGE('',*,*,#6914,.T.);
#9679=ORIENTED_EDGE('',*,*,#6901,.T.);
#9680=ORIENTED_EDGE('',*,*,#6914,.F.);
#9681=ORIENTED_EDGE('',*,*,#6915,.T.);
#9682=ORIENTED_EDGE('',*,*,#6916,.T.);
#9683=ORIENTED_EDGE('',*,*,#6902,.F.);
#9684=ORIENTED_EDGE('',*,*,#6916,.F.);
#9685=ORIENTED_EDGE('',*,*,#6917,.T.);
#9686=ORIENTED_EDGE('',*,*,#6918,.T.);
#9687=ORIENTED_EDGE('',*,*,#6903,.F.);
#9688=ORIENTED_EDGE('',*,*,#6918,.F.);
#9689=ORIENTED_EDGE('',*,*,#6919,.T.);
#9690=ORIENTED_EDGE('',*,*,#6920,.T.);
#9691=ORIENTED_EDGE('',*,*,#6904,.F.);
#9692=ORIENTED_EDGE('',*,*,#6920,.F.);
#9693=ORIENTED_EDGE('',*,*,#6921,.T.);
#9694=ORIENTED_EDGE('',*,*,#6922,.T.);
#9695=ORIENTED_EDGE('',*,*,#6905,.F.);
#9696=ORIENTED_EDGE('',*,*,#6922,.F.);
#9697=ORIENTED_EDGE('',*,*,#6923,.T.);
#9698=ORIENTED_EDGE('',*,*,#6924,.T.);
#9699=ORIENTED_EDGE('',*,*,#6906,.F.);
#9700=ORIENTED_EDGE('',*,*,#6924,.F.);
#9701=ORIENTED_EDGE('',*,*,#6925,.T.);
#9702=ORIENTED_EDGE('',*,*,#6926,.T.);
#9703=ORIENTED_EDGE('',*,*,#6907,.F.);
#9704=ORIENTED_EDGE('',*,*,#6926,.F.);
#9705=ORIENTED_EDGE('',*,*,#6927,.T.);
#9706=ORIENTED_EDGE('',*,*,#6928,.T.);
#9707=ORIENTED_EDGE('',*,*,#6908,.F.);
#9708=ORIENTED_EDGE('',*,*,#6928,.F.);
#9709=ORIENTED_EDGE('',*,*,#6929,.T.);
#9710=ORIENTED_EDGE('',*,*,#6930,.T.);
#9711=ORIENTED_EDGE('',*,*,#6909,.F.);
#9712=ORIENTED_EDGE('',*,*,#6930,.F.);
#9713=ORIENTED_EDGE('',*,*,#6931,.T.);
#9714=ORIENTED_EDGE('',*,*,#6932,.T.);
#9715=ORIENTED_EDGE('',*,*,#6898,.F.);
#9716=ORIENTED_EDGE('',*,*,#6932,.F.);
#9717=ORIENTED_EDGE('',*,*,#6933,.T.);
#9718=ORIENTED_EDGE('',*,*,#6910,.T.);
#9719=ORIENTED_EDGE('',*,*,#6899,.F.);
#9720=ORIENTED_EDGE('',*,*,#6931,.F.);
#9721=ORIENTED_EDGE('',*,*,#6929,.F.);
#9722=ORIENTED_EDGE('',*,*,#6927,.F.);
#9723=ORIENTED_EDGE('',*,*,#6925,.F.);
#9724=ORIENTED_EDGE('',*,*,#6923,.F.);
#9725=ORIENTED_EDGE('',*,*,#6921,.F.);
#9726=ORIENTED_EDGE('',*,*,#6919,.F.);
#9727=ORIENTED_EDGE('',*,*,#6917,.F.);
#9728=ORIENTED_EDGE('',*,*,#6915,.F.);
#9729=ORIENTED_EDGE('',*,*,#6913,.F.);
#9730=ORIENTED_EDGE('',*,*,#6911,.F.);
#9731=ORIENTED_EDGE('',*,*,#6933,.F.);
#9732=ORIENTED_EDGE('',*,*,#6934,.F.);
#9733=ORIENTED_EDGE('',*,*,#6935,.F.);
#9734=ORIENTED_EDGE('',*,*,#6936,.F.);
#9735=ORIENTED_EDGE('',*,*,#6937,.T.);
#9736=ORIENTED_EDGE('',*,*,#6938,.F.);
#9737=ORIENTED_EDGE('',*,*,#6939,.F.);
#9738=ORIENTED_EDGE('',*,*,#6940,.F.);
#9739=ORIENTED_EDGE('',*,*,#6935,.T.);
#9740=ORIENTED_EDGE('',*,*,#6941,.F.);
#9741=ORIENTED_EDGE('',*,*,#6942,.F.);
#9742=ORIENTED_EDGE('',*,*,#6943,.F.);
#9743=ORIENTED_EDGE('',*,*,#6939,.T.);
#9744=ORIENTED_EDGE('',*,*,#6944,.F.);
#9745=ORIENTED_EDGE('',*,*,#6945,.F.);
#9746=ORIENTED_EDGE('',*,*,#6946,.F.);
#9747=ORIENTED_EDGE('',*,*,#6942,.T.);
#9748=ORIENTED_EDGE('',*,*,#6947,.F.);
#9749=ORIENTED_EDGE('',*,*,#6948,.F.);
#9750=ORIENTED_EDGE('',*,*,#6949,.F.);
#9751=ORIENTED_EDGE('',*,*,#6945,.T.);
#9752=ORIENTED_EDGE('',*,*,#6950,.F.);
#9753=ORIENTED_EDGE('',*,*,#6951,.F.);
#9754=ORIENTED_EDGE('',*,*,#6952,.F.);
#9755=ORIENTED_EDGE('',*,*,#6948,.T.);
#9756=ORIENTED_EDGE('',*,*,#6953,.F.);
#9757=ORIENTED_EDGE('',*,*,#6954,.F.);
#9758=ORIENTED_EDGE('',*,*,#6955,.F.);
#9759=ORIENTED_EDGE('',*,*,#6951,.T.);
#9760=ORIENTED_EDGE('',*,*,#6956,.F.);
#9761=ORIENTED_EDGE('',*,*,#6957,.F.);
#9762=ORIENTED_EDGE('',*,*,#6958,.F.);
#9763=ORIENTED_EDGE('',*,*,#6954,.T.);
#9764=ORIENTED_EDGE('',*,*,#6959,.F.);
#9765=ORIENTED_EDGE('',*,*,#6960,.F.);
#9766=ORIENTED_EDGE('',*,*,#6961,.F.);
#9767=ORIENTED_EDGE('',*,*,#6957,.T.);
#9768=ORIENTED_EDGE('',*,*,#6962,.F.);
#9769=ORIENTED_EDGE('',*,*,#6963,.F.);
#9770=ORIENTED_EDGE('',*,*,#6964,.F.);
#9771=ORIENTED_EDGE('',*,*,#6960,.T.);
#9772=ORIENTED_EDGE('',*,*,#6965,.F.);
#9773=ORIENTED_EDGE('',*,*,#6966,.F.);
#9774=ORIENTED_EDGE('',*,*,#6967,.T.);
#9775=ORIENTED_EDGE('',*,*,#6963,.T.);
#9776=ORIENTED_EDGE('',*,*,#6968,.F.);
#9777=ORIENTED_EDGE('',*,*,#6937,.F.);
#9778=ORIENTED_EDGE('',*,*,#6969,.F.);
#9779=ORIENTED_EDGE('',*,*,#6966,.T.);
#9780=ORIENTED_EDGE('',*,*,#6940,.T.);
#9781=ORIENTED_EDGE('',*,*,#6943,.T.);
#9782=ORIENTED_EDGE('',*,*,#6946,.T.);
#9783=ORIENTED_EDGE('',*,*,#6949,.T.);
#9784=ORIENTED_EDGE('',*,*,#6952,.T.);
#9785=ORIENTED_EDGE('',*,*,#6955,.T.);
#9786=ORIENTED_EDGE('',*,*,#6958,.T.);
#9787=ORIENTED_EDGE('',*,*,#6961,.T.);
#9788=ORIENTED_EDGE('',*,*,#6964,.T.);
#9789=ORIENTED_EDGE('',*,*,#6967,.F.);
#9790=ORIENTED_EDGE('',*,*,#6969,.T.);
#9791=ORIENTED_EDGE('',*,*,#6936,.T.);
#9792=ORIENTED_EDGE('',*,*,#6938,.T.);
#9793=ORIENTED_EDGE('',*,*,#6934,.T.);
#9794=ORIENTED_EDGE('',*,*,#6968,.T.);
#9795=ORIENTED_EDGE('',*,*,#6965,.T.);
#9796=ORIENTED_EDGE('',*,*,#6962,.T.);
#9797=ORIENTED_EDGE('',*,*,#6959,.T.);
#9798=ORIENTED_EDGE('',*,*,#6956,.T.);
#9799=ORIENTED_EDGE('',*,*,#6953,.T.);
#9800=ORIENTED_EDGE('',*,*,#6950,.T.);
#9801=ORIENTED_EDGE('',*,*,#6947,.T.);
#9802=ORIENTED_EDGE('',*,*,#6944,.T.);
#9803=ORIENTED_EDGE('',*,*,#6941,.T.);
#9804=ORIENTED_EDGE('',*,*,#6970,.T.);
#9805=ORIENTED_EDGE('',*,*,#6971,.T.);
#9806=ORIENTED_EDGE('',*,*,#6972,.T.);
#9807=ORIENTED_EDGE('',*,*,#6973,.T.);
#9808=ORIENTED_EDGE('',*,*,#6974,.T.);
#9809=ORIENTED_EDGE('',*,*,#6975,.T.);
#9810=ORIENTED_EDGE('',*,*,#6976,.T.);
#9811=ORIENTED_EDGE('',*,*,#6977,.T.);
#9812=ORIENTED_EDGE('',*,*,#6978,.T.);
#9813=ORIENTED_EDGE('',*,*,#6979,.T.);
#9814=ORIENTED_EDGE('',*,*,#6980,.T.);
#9815=ORIENTED_EDGE('',*,*,#6981,.T.);
#9816=ORIENTED_EDGE('',*,*,#6982,.F.);
#9817=ORIENTED_EDGE('',*,*,#6983,.T.);
#9818=ORIENTED_EDGE('',*,*,#6984,.T.);
#9819=ORIENTED_EDGE('',*,*,#6972,.F.);
#9820=ORIENTED_EDGE('',*,*,#6984,.F.);
#9821=ORIENTED_EDGE('',*,*,#6985,.T.);
#9822=ORIENTED_EDGE('',*,*,#6986,.T.);
#9823=ORIENTED_EDGE('',*,*,#6973,.F.);
#9824=ORIENTED_EDGE('',*,*,#6986,.F.);
#9825=ORIENTED_EDGE('',*,*,#6987,.T.);
#9826=ORIENTED_EDGE('',*,*,#6988,.T.);
#9827=ORIENTED_EDGE('',*,*,#6974,.F.);
#9828=ORIENTED_EDGE('',*,*,#6988,.F.);
#9829=ORIENTED_EDGE('',*,*,#6989,.T.);
#9830=ORIENTED_EDGE('',*,*,#6990,.T.);
#9831=ORIENTED_EDGE('',*,*,#6975,.F.);
#9832=ORIENTED_EDGE('',*,*,#6990,.F.);
#9833=ORIENTED_EDGE('',*,*,#6991,.T.);
#9834=ORIENTED_EDGE('',*,*,#6992,.T.);
#9835=ORIENTED_EDGE('',*,*,#6976,.F.);
#9836=ORIENTED_EDGE('',*,*,#6992,.F.);
#9837=ORIENTED_EDGE('',*,*,#6993,.T.);
#9838=ORIENTED_EDGE('',*,*,#6994,.T.);
#9839=ORIENTED_EDGE('',*,*,#6977,.F.);
#9840=ORIENTED_EDGE('',*,*,#6994,.F.);
#9841=ORIENTED_EDGE('',*,*,#6995,.T.);
#9842=ORIENTED_EDGE('',*,*,#6996,.T.);
#9843=ORIENTED_EDGE('',*,*,#6978,.F.);
#9844=ORIENTED_EDGE('',*,*,#6996,.F.);
#9845=ORIENTED_EDGE('',*,*,#6997,.T.);
#9846=ORIENTED_EDGE('',*,*,#6998,.T.);
#9847=ORIENTED_EDGE('',*,*,#6979,.F.);
#9848=ORIENTED_EDGE('',*,*,#6998,.F.);
#9849=ORIENTED_EDGE('',*,*,#6999,.T.);
#9850=ORIENTED_EDGE('',*,*,#7000,.T.);
#9851=ORIENTED_EDGE('',*,*,#6980,.F.);
#9852=ORIENTED_EDGE('',*,*,#7000,.F.);
#9853=ORIENTED_EDGE('',*,*,#7001,.T.);
#9854=ORIENTED_EDGE('',*,*,#7002,.T.);
#9855=ORIENTED_EDGE('',*,*,#6981,.F.);
#9856=ORIENTED_EDGE('',*,*,#7002,.F.);
#9857=ORIENTED_EDGE('',*,*,#7003,.T.);
#9858=ORIENTED_EDGE('',*,*,#7004,.T.);
#9859=ORIENTED_EDGE('',*,*,#6970,.F.);
#9860=ORIENTED_EDGE('',*,*,#7004,.F.);
#9861=ORIENTED_EDGE('',*,*,#7005,.T.);
#9862=ORIENTED_EDGE('',*,*,#6982,.T.);
#9863=ORIENTED_EDGE('',*,*,#6971,.F.);
#9864=ORIENTED_EDGE('',*,*,#7003,.F.);
#9865=ORIENTED_EDGE('',*,*,#7001,.F.);
#9866=ORIENTED_EDGE('',*,*,#6999,.F.);
#9867=ORIENTED_EDGE('',*,*,#6997,.F.);
#9868=ORIENTED_EDGE('',*,*,#6995,.F.);
#9869=ORIENTED_EDGE('',*,*,#6993,.F.);
#9870=ORIENTED_EDGE('',*,*,#6991,.F.);
#9871=ORIENTED_EDGE('',*,*,#6989,.F.);
#9872=ORIENTED_EDGE('',*,*,#6987,.F.);
#9873=ORIENTED_EDGE('',*,*,#6985,.F.);
#9874=ORIENTED_EDGE('',*,*,#6983,.F.);
#9875=ORIENTED_EDGE('',*,*,#7005,.F.);
#9876=ORIENTED_EDGE('',*,*,#7006,.T.);
#9877=ORIENTED_EDGE('',*,*,#7007,.T.);
#9878=ORIENTED_EDGE('',*,*,#7008,.T.);
#9879=ORIENTED_EDGE('',*,*,#7009,.T.);
#9880=ORIENTED_EDGE('',*,*,#7010,.T.);
#9881=ORIENTED_EDGE('',*,*,#7011,.T.);
#9882=ORIENTED_EDGE('',*,*,#7012,.T.);
#9883=ORIENTED_EDGE('',*,*,#7013,.T.);
#9884=ORIENTED_EDGE('',*,*,#7014,.T.);
#9885=ORIENTED_EDGE('',*,*,#7015,.T.);
#9886=ORIENTED_EDGE('',*,*,#7016,.T.);
#9887=ORIENTED_EDGE('',*,*,#7017,.T.);
#9888=ORIENTED_EDGE('',*,*,#7018,.T.);
#9889=ORIENTED_EDGE('',*,*,#7019,.T.);
#9890=ORIENTED_EDGE('',*,*,#7020,.F.);
#9891=ORIENTED_EDGE('',*,*,#7017,.F.);
#9892=ORIENTED_EDGE('',*,*,#7021,.T.);
#9893=ORIENTED_EDGE('',*,*,#7022,.T.);
#9894=ORIENTED_EDGE('',*,*,#7018,.F.);
#9895=ORIENTED_EDGE('',*,*,#7016,.F.);
#9896=ORIENTED_EDGE('',*,*,#7023,.T.);
#9897=ORIENTED_EDGE('',*,*,#7024,.T.);
#9898=ORIENTED_EDGE('',*,*,#7021,.F.);
#9899=ORIENTED_EDGE('',*,*,#7015,.F.);
#9900=ORIENTED_EDGE('',*,*,#7025,.T.);
#9901=ORIENTED_EDGE('',*,*,#7026,.T.);
#9902=ORIENTED_EDGE('',*,*,#7023,.F.);
#9903=ORIENTED_EDGE('',*,*,#7014,.F.);
#9904=ORIENTED_EDGE('',*,*,#7027,.T.);
#9905=ORIENTED_EDGE('',*,*,#7028,.T.);
#9906=ORIENTED_EDGE('',*,*,#7025,.F.);
#9907=ORIENTED_EDGE('',*,*,#7013,.F.);
#9908=ORIENTED_EDGE('',*,*,#7029,.T.);
#9909=ORIENTED_EDGE('',*,*,#7030,.T.);
#9910=ORIENTED_EDGE('',*,*,#7027,.F.);
#9911=ORIENTED_EDGE('',*,*,#7012,.F.);
#9912=ORIENTED_EDGE('',*,*,#7031,.T.);
#9913=ORIENTED_EDGE('',*,*,#7032,.T.);
#9914=ORIENTED_EDGE('',*,*,#7029,.F.);
#9915=ORIENTED_EDGE('',*,*,#7011,.F.);
#9916=ORIENTED_EDGE('',*,*,#7033,.T.);
#9917=ORIENTED_EDGE('',*,*,#7034,.T.);
#9918=ORIENTED_EDGE('',*,*,#7031,.F.);
#9919=ORIENTED_EDGE('',*,*,#7010,.F.);
#9920=ORIENTED_EDGE('',*,*,#7035,.T.);
#9921=ORIENTED_EDGE('',*,*,#7036,.T.);
#9922=ORIENTED_EDGE('',*,*,#7033,.F.);
#9923=ORIENTED_EDGE('',*,*,#7009,.F.);
#9924=ORIENTED_EDGE('',*,*,#7037,.T.);
#9925=ORIENTED_EDGE('',*,*,#7038,.T.);
#9926=ORIENTED_EDGE('',*,*,#7035,.F.);
#9927=ORIENTED_EDGE('',*,*,#7008,.F.);
#9928=ORIENTED_EDGE('',*,*,#7039,.T.);
#9929=ORIENTED_EDGE('',*,*,#7040,.T.);
#9930=ORIENTED_EDGE('',*,*,#7037,.F.);
#9931=ORIENTED_EDGE('',*,*,#7007,.F.);
#9932=ORIENTED_EDGE('',*,*,#7020,.T.);
#9933=ORIENTED_EDGE('',*,*,#7041,.T.);
#9934=ORIENTED_EDGE('',*,*,#7039,.F.);
#9935=ORIENTED_EDGE('',*,*,#7006,.F.);
#9936=ORIENTED_EDGE('',*,*,#7019,.F.);
#9937=ORIENTED_EDGE('',*,*,#7022,.F.);
#9938=ORIENTED_EDGE('',*,*,#7024,.F.);
#9939=ORIENTED_EDGE('',*,*,#7026,.F.);
#9940=ORIENTED_EDGE('',*,*,#7028,.F.);
#9941=ORIENTED_EDGE('',*,*,#7030,.F.);
#9942=ORIENTED_EDGE('',*,*,#7032,.F.);
#9943=ORIENTED_EDGE('',*,*,#7034,.F.);
#9944=ORIENTED_EDGE('',*,*,#7036,.F.);
#9945=ORIENTED_EDGE('',*,*,#7038,.F.);
#9946=ORIENTED_EDGE('',*,*,#7040,.F.);
#9947=ORIENTED_EDGE('',*,*,#7041,.F.);
#9948=ORIENTED_EDGE('',*,*,#7042,.F.);
#9949=ORIENTED_EDGE('',*,*,#7043,.F.);
#9950=ORIENTED_EDGE('',*,*,#7044,.F.);
#9951=ORIENTED_EDGE('',*,*,#7045,.F.);
#9952=ORIENTED_EDGE('',*,*,#7046,.F.);
#9953=ORIENTED_EDGE('',*,*,#7047,.F.);
#9954=ORIENTED_EDGE('',*,*,#7048,.F.);
#9955=ORIENTED_EDGE('',*,*,#7049,.F.);
#9956=ORIENTED_EDGE('',*,*,#7050,.F.);
#9957=ORIENTED_EDGE('',*,*,#7051,.F.);
#9958=ORIENTED_EDGE('',*,*,#7052,.F.);
#9959=ORIENTED_EDGE('',*,*,#7053,.F.);
#9960=ORIENTED_EDGE('',*,*,#7054,.F.);
#9961=ORIENTED_EDGE('',*,*,#7055,.T.);
#9962=ORIENTED_EDGE('',*,*,#7056,.T.);
#9963=ORIENTED_EDGE('',*,*,#7043,.T.);
#9964=ORIENTED_EDGE('',*,*,#7056,.F.);
#9965=ORIENTED_EDGE('',*,*,#7057,.T.);
#9966=ORIENTED_EDGE('',*,*,#7058,.T.);
#9967=ORIENTED_EDGE('',*,*,#7044,.T.);
#9968=ORIENTED_EDGE('',*,*,#7058,.F.);
#9969=ORIENTED_EDGE('',*,*,#7059,.T.);
#9970=ORIENTED_EDGE('',*,*,#7060,.T.);
#9971=ORIENTED_EDGE('',*,*,#7045,.T.);
#9972=ORIENTED_EDGE('',*,*,#7060,.F.);
#9973=ORIENTED_EDGE('',*,*,#7061,.T.);
#9974=ORIENTED_EDGE('',*,*,#7062,.T.);
#9975=ORIENTED_EDGE('',*,*,#7046,.T.);
#9976=ORIENTED_EDGE('',*,*,#7062,.F.);
#9977=ORIENTED_EDGE('',*,*,#7063,.T.);
#9978=ORIENTED_EDGE('',*,*,#7064,.T.);
#9979=ORIENTED_EDGE('',*,*,#7047,.T.);
#9980=ORIENTED_EDGE('',*,*,#7064,.F.);
#9981=ORIENTED_EDGE('',*,*,#7065,.T.);
#9982=ORIENTED_EDGE('',*,*,#7066,.T.);
#9983=ORIENTED_EDGE('',*,*,#7048,.T.);
#9984=ORIENTED_EDGE('',*,*,#7066,.F.);
#9985=ORIENTED_EDGE('',*,*,#7067,.T.);
#9986=ORIENTED_EDGE('',*,*,#7068,.T.);
#9987=ORIENTED_EDGE('',*,*,#7049,.T.);
#9988=ORIENTED_EDGE('',*,*,#7068,.F.);
#9989=ORIENTED_EDGE('',*,*,#7069,.T.);
#9990=ORIENTED_EDGE('',*,*,#7070,.T.);
#9991=ORIENTED_EDGE('',*,*,#7050,.T.);
#9992=ORIENTED_EDGE('',*,*,#7070,.F.);
#9993=ORIENTED_EDGE('',*,*,#7071,.T.);
#9994=ORIENTED_EDGE('',*,*,#7072,.T.);
#9995=ORIENTED_EDGE('',*,*,#7051,.T.);
#9996=ORIENTED_EDGE('',*,*,#7072,.F.);
#9997=ORIENTED_EDGE('',*,*,#7073,.T.);
#9998=ORIENTED_EDGE('',*,*,#7074,.T.);
#9999=ORIENTED_EDGE('',*,*,#7052,.T.);
#10000=ORIENTED_EDGE('',*,*,#7074,.F.);
#10001=ORIENTED_EDGE('',*,*,#7075,.T.);
#10002=ORIENTED_EDGE('',*,*,#7076,.T.);
#10003=ORIENTED_EDGE('',*,*,#7053,.T.);
#10004=ORIENTED_EDGE('',*,*,#7076,.F.);
#10005=ORIENTED_EDGE('',*,*,#7077,.T.);
#10006=ORIENTED_EDGE('',*,*,#7054,.T.);
#10007=ORIENTED_EDGE('',*,*,#7042,.T.);
#10008=ORIENTED_EDGE('',*,*,#7075,.F.);
#10009=ORIENTED_EDGE('',*,*,#7073,.F.);
#10010=ORIENTED_EDGE('',*,*,#7071,.F.);
#10011=ORIENTED_EDGE('',*,*,#7069,.F.);
#10012=ORIENTED_EDGE('',*,*,#7067,.F.);
#10013=ORIENTED_EDGE('',*,*,#7065,.F.);
#10014=ORIENTED_EDGE('',*,*,#7063,.F.);
#10015=ORIENTED_EDGE('',*,*,#7061,.F.);
#10016=ORIENTED_EDGE('',*,*,#7059,.F.);
#10017=ORIENTED_EDGE('',*,*,#7057,.F.);
#10018=ORIENTED_EDGE('',*,*,#7055,.F.);
#10019=ORIENTED_EDGE('',*,*,#7077,.F.);
#10020=ORIENTED_EDGE('',*,*,#7078,.T.);
#10021=ORIENTED_EDGE('',*,*,#7079,.F.);
#10022=ORIENTED_EDGE('',*,*,#7080,.F.);
#10023=ORIENTED_EDGE('',*,*,#7081,.T.);
#10024=ORIENTED_EDGE('',*,*,#7082,.T.);
#10025=ORIENTED_EDGE('',*,*,#7083,.F.);
#10026=ORIENTED_EDGE('',*,*,#7084,.F.);
#10027=ORIENTED_EDGE('',*,*,#7079,.T.);
#10028=ORIENTED_EDGE('',*,*,#7085,.T.);
#10029=ORIENTED_EDGE('',*,*,#7086,.F.);
#10030=ORIENTED_EDGE('',*,*,#7087,.F.);
#10031=ORIENTED_EDGE('',*,*,#7083,.T.);
#10032=ORIENTED_EDGE('',*,*,#7088,.T.);
#10033=ORIENTED_EDGE('',*,*,#7089,.F.);
#10034=ORIENTED_EDGE('',*,*,#7090,.F.);
#10035=ORIENTED_EDGE('',*,*,#7086,.T.);
#10036=ORIENTED_EDGE('',*,*,#7091,.T.);
#10037=ORIENTED_EDGE('',*,*,#7092,.F.);
#10038=ORIENTED_EDGE('',*,*,#7093,.F.);
#10039=ORIENTED_EDGE('',*,*,#7089,.T.);
#10040=ORIENTED_EDGE('',*,*,#7094,.T.);
#10041=ORIENTED_EDGE('',*,*,#7095,.F.);
#10042=ORIENTED_EDGE('',*,*,#7096,.F.);
#10043=ORIENTED_EDGE('',*,*,#7092,.T.);
#10044=ORIENTED_EDGE('',*,*,#7097,.T.);
#10045=ORIENTED_EDGE('',*,*,#7098,.F.);
#10046=ORIENTED_EDGE('',*,*,#7099,.F.);
#10047=ORIENTED_EDGE('',*,*,#7095,.T.);
#10048=ORIENTED_EDGE('',*,*,#7100,.T.);
#10049=ORIENTED_EDGE('',*,*,#7101,.F.);
#10050=ORIENTED_EDGE('',*,*,#7102,.F.);
#10051=ORIENTED_EDGE('',*,*,#7098,.T.);
#10052=ORIENTED_EDGE('',*,*,#7103,.T.);
#10053=ORIENTED_EDGE('',*,*,#7081,.F.);
#10054=ORIENTED_EDGE('',*,*,#7104,.F.);
#10055=ORIENTED_EDGE('',*,*,#7101,.T.);
#10056=ORIENTED_EDGE('',*,*,#7080,.T.);
#10057=ORIENTED_EDGE('',*,*,#7084,.T.);
#10058=ORIENTED_EDGE('',*,*,#7087,.T.);
#10059=ORIENTED_EDGE('',*,*,#7090,.T.);
#10060=ORIENTED_EDGE('',*,*,#7093,.T.);
#10061=ORIENTED_EDGE('',*,*,#7096,.T.);
#10062=ORIENTED_EDGE('',*,*,#7099,.T.);
#10063=ORIENTED_EDGE('',*,*,#7102,.T.);
#10064=ORIENTED_EDGE('',*,*,#7104,.T.);
#10065=ORIENTED_EDGE('',*,*,#7078,.F.);
#10066=ORIENTED_EDGE('',*,*,#7103,.F.);
#10067=ORIENTED_EDGE('',*,*,#7100,.F.);
#10068=ORIENTED_EDGE('',*,*,#7097,.F.);
#10069=ORIENTED_EDGE('',*,*,#7094,.F.);
#10070=ORIENTED_EDGE('',*,*,#7091,.F.);
#10071=ORIENTED_EDGE('',*,*,#7088,.F.);
#10072=ORIENTED_EDGE('',*,*,#7085,.F.);
#10073=ORIENTED_EDGE('',*,*,#7082,.F.);
#10074=ORIENTED_EDGE('',*,*,#7105,.T.);
#10075=ORIENTED_EDGE('',*,*,#7106,.F.);
#10076=ORIENTED_EDGE('',*,*,#7107,.F.);
#10077=ORIENTED_EDGE('',*,*,#7108,.T.);
#10078=ORIENTED_EDGE('',*,*,#7109,.T.);
#10079=ORIENTED_EDGE('',*,*,#7110,.F.);
#10080=ORIENTED_EDGE('',*,*,#7111,.F.);
#10081=ORIENTED_EDGE('',*,*,#7106,.T.);
#10082=ORIENTED_EDGE('',*,*,#7112,.T.);
#10083=ORIENTED_EDGE('',*,*,#7113,.F.);
#10084=ORIENTED_EDGE('',*,*,#7114,.F.);
#10085=ORIENTED_EDGE('',*,*,#7110,.T.);
#10086=ORIENTED_EDGE('',*,*,#7115,.T.);
#10087=ORIENTED_EDGE('',*,*,#7116,.F.);
#10088=ORIENTED_EDGE('',*,*,#7117,.F.);
#10089=ORIENTED_EDGE('',*,*,#7113,.T.);
#10090=ORIENTED_EDGE('',*,*,#7118,.T.);
#10091=ORIENTED_EDGE('',*,*,#7119,.F.);
#10092=ORIENTED_EDGE('',*,*,#7120,.F.);
#10093=ORIENTED_EDGE('',*,*,#7116,.T.);
#10094=ORIENTED_EDGE('',*,*,#7121,.T.);
#10095=ORIENTED_EDGE('',*,*,#7122,.F.);
#10096=ORIENTED_EDGE('',*,*,#7123,.F.);
#10097=ORIENTED_EDGE('',*,*,#7119,.T.);
#10098=ORIENTED_EDGE('',*,*,#7124,.T.);
#10099=ORIENTED_EDGE('',*,*,#7125,.F.);
#10100=ORIENTED_EDGE('',*,*,#7126,.F.);
#10101=ORIENTED_EDGE('',*,*,#7122,.T.);
#10102=ORIENTED_EDGE('',*,*,#7127,.T.);
#10103=ORIENTED_EDGE('',*,*,#7128,.F.);
#10104=ORIENTED_EDGE('',*,*,#7129,.F.);
#10105=ORIENTED_EDGE('',*,*,#7125,.T.);
#10106=ORIENTED_EDGE('',*,*,#7130,.T.);
#10107=ORIENTED_EDGE('',*,*,#7108,.F.);
#10108=ORIENTED_EDGE('',*,*,#7131,.F.);
#10109=ORIENTED_EDGE('',*,*,#7128,.T.);
#10110=ORIENTED_EDGE('',*,*,#7107,.T.);
#10111=ORIENTED_EDGE('',*,*,#7111,.T.);
#10112=ORIENTED_EDGE('',*,*,#7114,.T.);
#10113=ORIENTED_EDGE('',*,*,#7117,.T.);
#10114=ORIENTED_EDGE('',*,*,#7120,.T.);
#10115=ORIENTED_EDGE('',*,*,#7123,.T.);
#10116=ORIENTED_EDGE('',*,*,#7126,.T.);
#10117=ORIENTED_EDGE('',*,*,#7129,.T.);
#10118=ORIENTED_EDGE('',*,*,#7131,.T.);
#10119=ORIENTED_EDGE('',*,*,#7105,.F.);
#10120=ORIENTED_EDGE('',*,*,#7130,.F.);
#10121=ORIENTED_EDGE('',*,*,#7127,.F.);
#10122=ORIENTED_EDGE('',*,*,#7124,.F.);
#10123=ORIENTED_EDGE('',*,*,#7121,.F.);
#10124=ORIENTED_EDGE('',*,*,#7118,.F.);
#10125=ORIENTED_EDGE('',*,*,#7115,.F.);
#10126=ORIENTED_EDGE('',*,*,#7112,.F.);
#10127=ORIENTED_EDGE('',*,*,#7109,.F.);
#10128=ORIENTED_EDGE('',*,*,#7132,.F.);
#10129=ORIENTED_EDGE('',*,*,#7133,.F.);
#10130=ORIENTED_EDGE('',*,*,#7134,.T.);
#10131=ORIENTED_EDGE('',*,*,#7135,.T.);
#10132=ORIENTED_EDGE('',*,*,#7136,.F.);
#10133=ORIENTED_EDGE('',*,*,#7135,.F.);
#10134=ORIENTED_EDGE('',*,*,#7137,.T.);
#10135=ORIENTED_EDGE('',*,*,#7138,.T.);
#10136=ORIENTED_EDGE('',*,*,#7139,.F.);
#10137=ORIENTED_EDGE('',*,*,#7138,.F.);
#10138=ORIENTED_EDGE('',*,*,#7140,.T.);
#10139=ORIENTED_EDGE('',*,*,#7141,.T.);
#10140=ORIENTED_EDGE('',*,*,#7142,.F.);
#10141=ORIENTED_EDGE('',*,*,#7141,.F.);
#10142=ORIENTED_EDGE('',*,*,#7143,.T.);
#10143=ORIENTED_EDGE('',*,*,#7144,.T.);
#10144=ORIENTED_EDGE('',*,*,#7145,.F.);
#10145=ORIENTED_EDGE('',*,*,#7144,.F.);
#10146=ORIENTED_EDGE('',*,*,#7146,.T.);
#10147=ORIENTED_EDGE('',*,*,#7147,.T.);
#10148=ORIENTED_EDGE('',*,*,#7148,.F.);
#10149=ORIENTED_EDGE('',*,*,#7147,.F.);
#10150=ORIENTED_EDGE('',*,*,#7149,.T.);
#10151=ORIENTED_EDGE('',*,*,#7150,.T.);
#10152=ORIENTED_EDGE('',*,*,#7151,.F.);
#10153=ORIENTED_EDGE('',*,*,#7150,.F.);
#10154=ORIENTED_EDGE('',*,*,#7152,.T.);
#10155=ORIENTED_EDGE('',*,*,#7153,.T.);
#10156=ORIENTED_EDGE('',*,*,#7154,.F.);
#10157=ORIENTED_EDGE('',*,*,#7153,.F.);
#10158=ORIENTED_EDGE('',*,*,#7155,.T.);
#10159=ORIENTED_EDGE('',*,*,#7156,.T.);
#10160=ORIENTED_EDGE('',*,*,#7157,.F.);
#10161=ORIENTED_EDGE('',*,*,#7156,.F.);
#10162=ORIENTED_EDGE('',*,*,#7158,.T.);
#10163=ORIENTED_EDGE('',*,*,#7133,.T.);
#10164=ORIENTED_EDGE('',*,*,#7134,.F.);
#10165=ORIENTED_EDGE('',*,*,#7158,.F.);
#10166=ORIENTED_EDGE('',*,*,#7155,.F.);
#10167=ORIENTED_EDGE('',*,*,#7152,.F.);
#10168=ORIENTED_EDGE('',*,*,#7149,.F.);
#10169=ORIENTED_EDGE('',*,*,#7146,.F.);
#10170=ORIENTED_EDGE('',*,*,#7143,.F.);
#10171=ORIENTED_EDGE('',*,*,#7140,.F.);
#10172=ORIENTED_EDGE('',*,*,#7137,.F.);
#10173=ORIENTED_EDGE('',*,*,#7132,.T.);
#10174=ORIENTED_EDGE('',*,*,#7136,.T.);
#10175=ORIENTED_EDGE('',*,*,#7139,.T.);
#10176=ORIENTED_EDGE('',*,*,#7142,.T.);
#10177=ORIENTED_EDGE('',*,*,#7145,.T.);
#10178=ORIENTED_EDGE('',*,*,#7148,.T.);
#10179=ORIENTED_EDGE('',*,*,#7151,.T.);
#10180=ORIENTED_EDGE('',*,*,#7154,.T.);
#10181=ORIENTED_EDGE('',*,*,#7157,.T.);
#10182=ORIENTED_EDGE('',*,*,#7159,.F.);
#10183=ORIENTED_EDGE('',*,*,#7160,.F.);
#10184=ORIENTED_EDGE('',*,*,#7161,.T.);
#10185=ORIENTED_EDGE('',*,*,#7162,.T.);
#10186=ORIENTED_EDGE('',*,*,#7163,.F.);
#10187=ORIENTED_EDGE('',*,*,#7162,.F.);
#10188=ORIENTED_EDGE('',*,*,#7164,.T.);
#10189=ORIENTED_EDGE('',*,*,#7165,.T.);
#10190=ORIENTED_EDGE('',*,*,#7166,.F.);
#10191=ORIENTED_EDGE('',*,*,#7165,.F.);
#10192=ORIENTED_EDGE('',*,*,#7167,.T.);
#10193=ORIENTED_EDGE('',*,*,#7168,.T.);
#10194=ORIENTED_EDGE('',*,*,#7169,.F.);
#10195=ORIENTED_EDGE('',*,*,#7168,.F.);
#10196=ORIENTED_EDGE('',*,*,#7170,.T.);
#10197=ORIENTED_EDGE('',*,*,#7171,.T.);
#10198=ORIENTED_EDGE('',*,*,#7172,.F.);
#10199=ORIENTED_EDGE('',*,*,#7171,.F.);
#10200=ORIENTED_EDGE('',*,*,#7173,.T.);
#10201=ORIENTED_EDGE('',*,*,#7174,.T.);
#10202=ORIENTED_EDGE('',*,*,#7175,.F.);
#10203=ORIENTED_EDGE('',*,*,#7174,.F.);
#10204=ORIENTED_EDGE('',*,*,#7176,.T.);
#10205=ORIENTED_EDGE('',*,*,#7177,.T.);
#10206=ORIENTED_EDGE('',*,*,#7178,.F.);
#10207=ORIENTED_EDGE('',*,*,#7177,.F.);
#10208=ORIENTED_EDGE('',*,*,#7179,.T.);
#10209=ORIENTED_EDGE('',*,*,#7180,.T.);
#10210=ORIENTED_EDGE('',*,*,#7181,.F.);
#10211=ORIENTED_EDGE('',*,*,#7180,.F.);
#10212=ORIENTED_EDGE('',*,*,#7182,.T.);
#10213=ORIENTED_EDGE('',*,*,#7183,.T.);
#10214=ORIENTED_EDGE('',*,*,#7184,.F.);
#10215=ORIENTED_EDGE('',*,*,#7183,.F.);
#10216=ORIENTED_EDGE('',*,*,#7185,.T.);
#10217=ORIENTED_EDGE('',*,*,#7160,.T.);
#10218=ORIENTED_EDGE('',*,*,#7161,.F.);
#10219=ORIENTED_EDGE('',*,*,#7185,.F.);
#10220=ORIENTED_EDGE('',*,*,#7182,.F.);
#10221=ORIENTED_EDGE('',*,*,#7179,.F.);
#10222=ORIENTED_EDGE('',*,*,#7176,.F.);
#10223=ORIENTED_EDGE('',*,*,#7173,.F.);
#10224=ORIENTED_EDGE('',*,*,#7170,.F.);
#10225=ORIENTED_EDGE('',*,*,#7167,.F.);
#10226=ORIENTED_EDGE('',*,*,#7164,.F.);
#10227=ORIENTED_EDGE('',*,*,#7159,.T.);
#10228=ORIENTED_EDGE('',*,*,#7163,.T.);
#10229=ORIENTED_EDGE('',*,*,#7166,.T.);
#10230=ORIENTED_EDGE('',*,*,#7169,.T.);
#10231=ORIENTED_EDGE('',*,*,#7172,.T.);
#10232=ORIENTED_EDGE('',*,*,#7175,.T.);
#10233=ORIENTED_EDGE('',*,*,#7178,.T.);
#10234=ORIENTED_EDGE('',*,*,#7181,.T.);
#10235=ORIENTED_EDGE('',*,*,#7184,.T.);
#10236=ORIENTED_EDGE('',*,*,#7186,.T.);
#10237=ORIENTED_EDGE('',*,*,#7187,.T.);
#10238=ORIENTED_EDGE('',*,*,#7188,.T.);
#10239=ORIENTED_EDGE('',*,*,#7189,.T.);
#10240=ORIENTED_EDGE('',*,*,#7190,.T.);
#10241=ORIENTED_EDGE('',*,*,#7191,.T.);
#10242=ORIENTED_EDGE('',*,*,#7192,.T.);
#10243=ORIENTED_EDGE('',*,*,#7193,.T.);
#10244=ORIENTED_EDGE('',*,*,#7194,.T.);
#10245=ORIENTED_EDGE('',*,*,#7195,.T.);
#10246=ORIENTED_EDGE('',*,*,#7196,.T.);
#10247=ORIENTED_EDGE('',*,*,#7197,.F.);
#10248=ORIENTED_EDGE('',*,*,#7194,.F.);
#10249=ORIENTED_EDGE('',*,*,#7198,.T.);
#10250=ORIENTED_EDGE('',*,*,#7199,.T.);
#10251=ORIENTED_EDGE('',*,*,#7195,.F.);
#10252=ORIENTED_EDGE('',*,*,#7193,.F.);
#10253=ORIENTED_EDGE('',*,*,#7200,.T.);
#10254=ORIENTED_EDGE('',*,*,#7201,.T.);
#10255=ORIENTED_EDGE('',*,*,#7198,.F.);
#10256=ORIENTED_EDGE('',*,*,#7192,.F.);
#10257=ORIENTED_EDGE('',*,*,#7202,.T.);
#10258=ORIENTED_EDGE('',*,*,#7203,.T.);
#10259=ORIENTED_EDGE('',*,*,#7200,.F.);
#10260=ORIENTED_EDGE('',*,*,#7191,.F.);
#10261=ORIENTED_EDGE('',*,*,#7204,.T.);
#10262=ORIENTED_EDGE('',*,*,#7205,.T.);
#10263=ORIENTED_EDGE('',*,*,#7202,.F.);
#10264=ORIENTED_EDGE('',*,*,#7190,.F.);
#10265=ORIENTED_EDGE('',*,*,#7206,.T.);
#10266=ORIENTED_EDGE('',*,*,#7207,.T.);
#10267=ORIENTED_EDGE('',*,*,#7204,.F.);
#10268=ORIENTED_EDGE('',*,*,#7189,.F.);
#10269=ORIENTED_EDGE('',*,*,#7208,.T.);
#10270=ORIENTED_EDGE('',*,*,#7209,.T.);
#10271=ORIENTED_EDGE('',*,*,#7206,.F.);
#10272=ORIENTED_EDGE('',*,*,#7188,.F.);
#10273=ORIENTED_EDGE('',*,*,#7210,.T.);
#10274=ORIENTED_EDGE('',*,*,#7211,.T.);
#10275=ORIENTED_EDGE('',*,*,#7208,.F.);
#10276=ORIENTED_EDGE('',*,*,#7187,.F.);
#10277=ORIENTED_EDGE('',*,*,#7197,.T.);
#10278=ORIENTED_EDGE('',*,*,#7212,.T.);
#10279=ORIENTED_EDGE('',*,*,#7210,.F.);
#10280=ORIENTED_EDGE('',*,*,#7186,.F.);
#10281=ORIENTED_EDGE('',*,*,#7196,.F.);
#10282=ORIENTED_EDGE('',*,*,#7199,.F.);
#10283=ORIENTED_EDGE('',*,*,#7201,.F.);
#10284=ORIENTED_EDGE('',*,*,#7203,.F.);
#10285=ORIENTED_EDGE('',*,*,#7205,.F.);
#10286=ORIENTED_EDGE('',*,*,#7207,.F.);
#10287=ORIENTED_EDGE('',*,*,#7209,.F.);
#10288=ORIENTED_EDGE('',*,*,#7211,.F.);
#10289=ORIENTED_EDGE('',*,*,#7212,.F.);
#10290=ORIENTED_EDGE('',*,*,#7213,.F.);
#10291=ORIENTED_EDGE('',*,*,#7214,.F.);
#10292=ORIENTED_EDGE('',*,*,#7215,.F.);
#10293=ORIENTED_EDGE('',*,*,#7216,.T.);
#10294=ORIENTED_EDGE('',*,*,#7217,.F.);
#10295=ORIENTED_EDGE('',*,*,#7218,.F.);
#10296=ORIENTED_EDGE('',*,*,#7219,.F.);
#10297=ORIENTED_EDGE('',*,*,#7214,.T.);
#10298=ORIENTED_EDGE('',*,*,#7220,.F.);
#10299=ORIENTED_EDGE('',*,*,#7221,.F.);
#10300=ORIENTED_EDGE('',*,*,#7222,.F.);
#10301=ORIENTED_EDGE('',*,*,#7218,.T.);
#10302=ORIENTED_EDGE('',*,*,#7223,.F.);
#10303=ORIENTED_EDGE('',*,*,#7224,.F.);
#10304=ORIENTED_EDGE('',*,*,#7225,.F.);
#10305=ORIENTED_EDGE('',*,*,#7221,.T.);
#10306=ORIENTED_EDGE('',*,*,#7226,.F.);
#10307=ORIENTED_EDGE('',*,*,#7227,.F.);
#10308=ORIENTED_EDGE('',*,*,#7228,.F.);
#10309=ORIENTED_EDGE('',*,*,#7224,.T.);
#10310=ORIENTED_EDGE('',*,*,#7229,.F.);
#10311=ORIENTED_EDGE('',*,*,#7230,.F.);
#10312=ORIENTED_EDGE('',*,*,#7231,.F.);
#10313=ORIENTED_EDGE('',*,*,#7227,.T.);
#10314=ORIENTED_EDGE('',*,*,#7232,.F.);
#10315=ORIENTED_EDGE('',*,*,#7233,.F.);
#10316=ORIENTED_EDGE('',*,*,#7234,.F.);
#10317=ORIENTED_EDGE('',*,*,#7230,.T.);
#10318=ORIENTED_EDGE('',*,*,#7235,.F.);
#10319=ORIENTED_EDGE('',*,*,#7236,.F.);
#10320=ORIENTED_EDGE('',*,*,#7237,.F.);
#10321=ORIENTED_EDGE('',*,*,#7233,.T.);
#10322=ORIENTED_EDGE('',*,*,#7238,.F.);
#10323=ORIENTED_EDGE('',*,*,#7216,.F.);
#10324=ORIENTED_EDGE('',*,*,#7239,.F.);
#10325=ORIENTED_EDGE('',*,*,#7236,.T.);
#10326=ORIENTED_EDGE('',*,*,#7239,.T.);
#10327=ORIENTED_EDGE('',*,*,#7215,.T.);
#10328=ORIENTED_EDGE('',*,*,#7219,.T.);
#10329=ORIENTED_EDGE('',*,*,#7222,.T.);
#10330=ORIENTED_EDGE('',*,*,#7225,.T.);
#10331=ORIENTED_EDGE('',*,*,#7228,.T.);
#10332=ORIENTED_EDGE('',*,*,#7231,.T.);
#10333=ORIENTED_EDGE('',*,*,#7234,.T.);
#10334=ORIENTED_EDGE('',*,*,#7237,.T.);
#10335=ORIENTED_EDGE('',*,*,#7217,.T.);
#10336=ORIENTED_EDGE('',*,*,#7213,.T.);
#10337=ORIENTED_EDGE('',*,*,#7238,.T.);
#10338=ORIENTED_EDGE('',*,*,#7235,.T.);
#10339=ORIENTED_EDGE('',*,*,#7232,.T.);
#10340=ORIENTED_EDGE('',*,*,#7229,.T.);
#10341=ORIENTED_EDGE('',*,*,#7226,.T.);
#10342=ORIENTED_EDGE('',*,*,#7223,.T.);
#10343=ORIENTED_EDGE('',*,*,#7220,.T.);
#10344=ORIENTED_EDGE('',*,*,#7240,.F.);
#10345=ORIENTED_EDGE('',*,*,#7241,.F.);
#10346=ORIENTED_EDGE('',*,*,#7242,.F.);
#10347=ORIENTED_EDGE('',*,*,#7243,.F.);
#10348=ORIENTED_EDGE('',*,*,#7244,.F.);
#10349=ORIENTED_EDGE('',*,*,#7245,.F.);
#10350=ORIENTED_EDGE('',*,*,#7246,.F.);
#10351=ORIENTED_EDGE('',*,*,#7247,.F.);
#10352=ORIENTED_EDGE('',*,*,#7248,.F.);
#10353=ORIENTED_EDGE('',*,*,#7249,.F.);
#10354=ORIENTED_EDGE('',*,*,#7250,.T.);
#10355=ORIENTED_EDGE('',*,*,#7251,.T.);
#10356=ORIENTED_EDGE('',*,*,#7241,.T.);
#10357=ORIENTED_EDGE('',*,*,#7251,.F.);
#10358=ORIENTED_EDGE('',*,*,#7252,.T.);
#10359=ORIENTED_EDGE('',*,*,#7253,.T.);
#10360=ORIENTED_EDGE('',*,*,#7242,.T.);
#10361=ORIENTED_EDGE('',*,*,#7253,.F.);
#10362=ORIENTED_EDGE('',*,*,#7254,.T.);
#10363=ORIENTED_EDGE('',*,*,#7255,.T.);
#10364=ORIENTED_EDGE('',*,*,#7243,.T.);
#10365=ORIENTED_EDGE('',*,*,#7255,.F.);
#10366=ORIENTED_EDGE('',*,*,#7256,.T.);
#10367=ORIENTED_EDGE('',*,*,#7257,.T.);
#10368=ORIENTED_EDGE('',*,*,#7244,.T.);
#10369=ORIENTED_EDGE('',*,*,#7257,.F.);
#10370=ORIENTED_EDGE('',*,*,#7258,.T.);
#10371=ORIENTED_EDGE('',*,*,#7259,.T.);
#10372=ORIENTED_EDGE('',*,*,#7245,.T.);
#10373=ORIENTED_EDGE('',*,*,#7259,.F.);
#10374=ORIENTED_EDGE('',*,*,#7260,.T.);
#10375=ORIENTED_EDGE('',*,*,#7261,.T.);
#10376=ORIENTED_EDGE('',*,*,#7246,.T.);
#10377=ORIENTED_EDGE('',*,*,#7261,.F.);
#10378=ORIENTED_EDGE('',*,*,#7262,.T.);
#10379=ORIENTED_EDGE('',*,*,#7263,.T.);
#10380=ORIENTED_EDGE('',*,*,#7247,.T.);
#10381=ORIENTED_EDGE('',*,*,#7263,.F.);
#10382=ORIENTED_EDGE('',*,*,#7264,.T.);
#10383=ORIENTED_EDGE('',*,*,#7265,.T.);
#10384=ORIENTED_EDGE('',*,*,#7248,.T.);
#10385=ORIENTED_EDGE('',*,*,#7265,.F.);
#10386=ORIENTED_EDGE('',*,*,#7266,.T.);
#10387=ORIENTED_EDGE('',*,*,#7249,.T.);
#10388=ORIENTED_EDGE('',*,*,#7240,.T.);
#10389=ORIENTED_EDGE('',*,*,#7264,.F.);
#10390=ORIENTED_EDGE('',*,*,#7262,.F.);
#10391=ORIENTED_EDGE('',*,*,#7260,.F.);
#10392=ORIENTED_EDGE('',*,*,#7258,.F.);
#10393=ORIENTED_EDGE('',*,*,#7256,.F.);
#10394=ORIENTED_EDGE('',*,*,#7254,.F.);
#10395=ORIENTED_EDGE('',*,*,#7252,.F.);
#10396=ORIENTED_EDGE('',*,*,#7250,.F.);
#10397=ORIENTED_EDGE('',*,*,#7266,.F.);
#10398=ORIENTED_EDGE('',*,*,#7267,.F.);
#10399=ORIENTED_EDGE('',*,*,#7268,.F.);
#10400=ORIENTED_EDGE('',*,*,#7269,.F.);
#10401=ORIENTED_EDGE('',*,*,#7270,.F.);
#10402=ORIENTED_EDGE('',*,*,#7271,.F.);
#10403=ORIENTED_EDGE('',*,*,#7272,.F.);
#10404=ORIENTED_EDGE('',*,*,#7273,.F.);
#10405=ORIENTED_EDGE('',*,*,#7274,.F.);
#10406=ORIENTED_EDGE('',*,*,#7275,.F.);
#10407=ORIENTED_EDGE('',*,*,#7276,.F.);
#10408=ORIENTED_EDGE('',*,*,#7277,.T.);
#10409=ORIENTED_EDGE('',*,*,#7278,.T.);
#10410=ORIENTED_EDGE('',*,*,#7268,.T.);
#10411=ORIENTED_EDGE('',*,*,#7278,.F.);
#10412=ORIENTED_EDGE('',*,*,#7279,.T.);
#10413=ORIENTED_EDGE('',*,*,#7280,.T.);
#10414=ORIENTED_EDGE('',*,*,#7269,.T.);
#10415=ORIENTED_EDGE('',*,*,#7280,.F.);
#10416=ORIENTED_EDGE('',*,*,#7281,.T.);
#10417=ORIENTED_EDGE('',*,*,#7282,.T.);
#10418=ORIENTED_EDGE('',*,*,#7270,.T.);
#10419=ORIENTED_EDGE('',*,*,#7282,.F.);
#10420=ORIENTED_EDGE('',*,*,#7283,.T.);
#10421=ORIENTED_EDGE('',*,*,#7284,.T.);
#10422=ORIENTED_EDGE('',*,*,#7271,.T.);
#10423=ORIENTED_EDGE('',*,*,#7284,.F.);
#10424=ORIENTED_EDGE('',*,*,#7285,.T.);
#10425=ORIENTED_EDGE('',*,*,#7286,.T.);
#10426=ORIENTED_EDGE('',*,*,#7272,.T.);
#10427=ORIENTED_EDGE('',*,*,#7286,.F.);
#10428=ORIENTED_EDGE('',*,*,#7287,.T.);
#10429=ORIENTED_EDGE('',*,*,#7288,.T.);
#10430=ORIENTED_EDGE('',*,*,#7273,.T.);
#10431=ORIENTED_EDGE('',*,*,#7288,.F.);
#10432=ORIENTED_EDGE('',*,*,#7289,.T.);
#10433=ORIENTED_EDGE('',*,*,#7290,.T.);
#10434=ORIENTED_EDGE('',*,*,#7274,.T.);
#10435=ORIENTED_EDGE('',*,*,#7290,.F.);
#10436=ORIENTED_EDGE('',*,*,#7291,.T.);
#10437=ORIENTED_EDGE('',*,*,#7292,.T.);
#10438=ORIENTED_EDGE('',*,*,#7275,.T.);
#10439=ORIENTED_EDGE('',*,*,#7292,.F.);
#10440=ORIENTED_EDGE('',*,*,#7293,.T.);
#10441=ORIENTED_EDGE('',*,*,#7276,.T.);
#10442=ORIENTED_EDGE('',*,*,#7267,.T.);
#10443=ORIENTED_EDGE('',*,*,#7291,.F.);
#10444=ORIENTED_EDGE('',*,*,#7289,.F.);
#10445=ORIENTED_EDGE('',*,*,#7287,.F.);
#10446=ORIENTED_EDGE('',*,*,#7285,.F.);
#10447=ORIENTED_EDGE('',*,*,#7283,.F.);
#10448=ORIENTED_EDGE('',*,*,#7281,.F.);
#10449=ORIENTED_EDGE('',*,*,#7279,.F.);
#10450=ORIENTED_EDGE('',*,*,#7277,.F.);
#10451=ORIENTED_EDGE('',*,*,#7293,.F.);
#10452=ORIENTED_EDGE('',*,*,#7294,.F.);
#10453=ORIENTED_EDGE('',*,*,#7295,.T.);
#10454=ORIENTED_EDGE('',*,*,#7296,.F.);
#10455=ORIENTED_EDGE('',*,*,#7297,.F.);
#10456=ORIENTED_EDGE('',*,*,#7298,.F.);
#10457=ORIENTED_EDGE('',*,*,#7297,.T.);
#10458=ORIENTED_EDGE('',*,*,#7299,.F.);
#10459=ORIENTED_EDGE('',*,*,#7300,.F.);
#10460=ORIENTED_EDGE('',*,*,#7301,.F.);
#10461=ORIENTED_EDGE('',*,*,#7300,.T.);
#10462=ORIENTED_EDGE('',*,*,#7302,.F.);
#10463=ORIENTED_EDGE('',*,*,#7303,.F.);
#10464=ORIENTED_EDGE('',*,*,#7304,.F.);
#10465=ORIENTED_EDGE('',*,*,#7303,.T.);
#10466=ORIENTED_EDGE('',*,*,#7305,.F.);
#10467=ORIENTED_EDGE('',*,*,#7306,.F.);
#10468=ORIENTED_EDGE('',*,*,#7307,.F.);
#10469=ORIENTED_EDGE('',*,*,#7306,.T.);
#10470=ORIENTED_EDGE('',*,*,#7308,.F.);
#10471=ORIENTED_EDGE('',*,*,#7309,.F.);
#10472=ORIENTED_EDGE('',*,*,#7310,.F.);
#10473=ORIENTED_EDGE('',*,*,#7309,.T.);
#10474=ORIENTED_EDGE('',*,*,#7311,.F.);
#10475=ORIENTED_EDGE('',*,*,#7312,.F.);
#10476=ORIENTED_EDGE('',*,*,#7313,.F.);
#10477=ORIENTED_EDGE('',*,*,#7312,.T.);
#10478=ORIENTED_EDGE('',*,*,#7314,.F.);
#10479=ORIENTED_EDGE('',*,*,#7315,.F.);
#10480=ORIENTED_EDGE('',*,*,#7316,.F.);
#10481=ORIENTED_EDGE('',*,*,#7315,.T.);
#10482=ORIENTED_EDGE('',*,*,#7317,.F.);
#10483=ORIENTED_EDGE('',*,*,#7318,.F.);
#10484=ORIENTED_EDGE('',*,*,#7319,.F.);
#10485=ORIENTED_EDGE('',*,*,#7318,.T.);
#10486=ORIENTED_EDGE('',*,*,#7320,.F.);
#10487=ORIENTED_EDGE('',*,*,#7295,.F.);
#10488=ORIENTED_EDGE('',*,*,#7299,.T.);
#10489=ORIENTED_EDGE('',*,*,#7296,.T.);
#10490=ORIENTED_EDGE('',*,*,#7320,.T.);
#10491=ORIENTED_EDGE('',*,*,#7317,.T.);
#10492=ORIENTED_EDGE('',*,*,#7314,.T.);
#10493=ORIENTED_EDGE('',*,*,#7311,.T.);
#10494=ORIENTED_EDGE('',*,*,#7308,.T.);
#10495=ORIENTED_EDGE('',*,*,#7305,.T.);
#10496=ORIENTED_EDGE('',*,*,#7302,.T.);
#10497=ORIENTED_EDGE('',*,*,#7319,.T.);
#10498=ORIENTED_EDGE('',*,*,#7294,.T.);
#10499=ORIENTED_EDGE('',*,*,#7298,.T.);
#10500=ORIENTED_EDGE('',*,*,#7301,.T.);
#10501=ORIENTED_EDGE('',*,*,#7304,.T.);
#10502=ORIENTED_EDGE('',*,*,#7307,.T.);
#10503=ORIENTED_EDGE('',*,*,#7310,.T.);
#10504=ORIENTED_EDGE('',*,*,#7313,.T.);
#10505=ORIENTED_EDGE('',*,*,#7316,.T.);
#10506=ORIENTED_EDGE('',*,*,#7321,.T.);
#10507=ORIENTED_EDGE('',*,*,#7322,.T.);
#10508=ORIENTED_EDGE('',*,*,#7323,.T.);
#10509=ORIENTED_EDGE('',*,*,#7324,.T.);
#10510=ORIENTED_EDGE('',*,*,#7325,.T.);
#10511=ORIENTED_EDGE('',*,*,#7326,.T.);
#10512=ORIENTED_EDGE('',*,*,#7327,.T.);
#10513=ORIENTED_EDGE('',*,*,#7328,.T.);
#10514=ORIENTED_EDGE('',*,*,#7329,.T.);
#10515=ORIENTED_EDGE('',*,*,#7330,.T.);
#10516=ORIENTED_EDGE('',*,*,#7331,.T.);
#10517=ORIENTED_EDGE('',*,*,#7332,.F.);
#10518=ORIENTED_EDGE('',*,*,#7329,.F.);
#10519=ORIENTED_EDGE('',*,*,#7333,.T.);
#10520=ORIENTED_EDGE('',*,*,#7334,.T.);
#10521=ORIENTED_EDGE('',*,*,#7330,.F.);
#10522=ORIENTED_EDGE('',*,*,#7328,.F.);
#10523=ORIENTED_EDGE('',*,*,#7335,.T.);
#10524=ORIENTED_EDGE('',*,*,#7336,.T.);
#10525=ORIENTED_EDGE('',*,*,#7333,.F.);
#10526=ORIENTED_EDGE('',*,*,#7327,.F.);
#10527=ORIENTED_EDGE('',*,*,#7337,.T.);
#10528=ORIENTED_EDGE('',*,*,#7338,.T.);
#10529=ORIENTED_EDGE('',*,*,#7335,.F.);
#10530=ORIENTED_EDGE('',*,*,#7326,.F.);
#10531=ORIENTED_EDGE('',*,*,#7339,.T.);
#10532=ORIENTED_EDGE('',*,*,#7340,.T.);
#10533=ORIENTED_EDGE('',*,*,#7337,.F.);
#10534=ORIENTED_EDGE('',*,*,#7325,.F.);
#10535=ORIENTED_EDGE('',*,*,#7341,.T.);
#10536=ORIENTED_EDGE('',*,*,#7342,.T.);
#10537=ORIENTED_EDGE('',*,*,#7339,.F.);
#10538=ORIENTED_EDGE('',*,*,#7324,.F.);
#10539=ORIENTED_EDGE('',*,*,#7343,.T.);
#10540=ORIENTED_EDGE('',*,*,#7344,.T.);
#10541=ORIENTED_EDGE('',*,*,#7341,.F.);
#10542=ORIENTED_EDGE('',*,*,#7323,.F.);
#10543=ORIENTED_EDGE('',*,*,#7345,.T.);
#10544=ORIENTED_EDGE('',*,*,#7346,.T.);
#10545=ORIENTED_EDGE('',*,*,#7343,.F.);
#10546=ORIENTED_EDGE('',*,*,#7322,.F.);
#10547=ORIENTED_EDGE('',*,*,#7332,.T.);
#10548=ORIENTED_EDGE('',*,*,#7347,.T.);
#10549=ORIENTED_EDGE('',*,*,#7345,.F.);
#10550=ORIENTED_EDGE('',*,*,#7321,.F.);
#10551=ORIENTED_EDGE('',*,*,#7331,.F.);
#10552=ORIENTED_EDGE('',*,*,#7334,.F.);
#10553=ORIENTED_EDGE('',*,*,#7336,.F.);
#10554=ORIENTED_EDGE('',*,*,#7338,.F.);
#10555=ORIENTED_EDGE('',*,*,#7340,.F.);
#10556=ORIENTED_EDGE('',*,*,#7342,.F.);
#10557=ORIENTED_EDGE('',*,*,#7344,.F.);
#10558=ORIENTED_EDGE('',*,*,#7346,.F.);
#10559=ORIENTED_EDGE('',*,*,#7347,.F.);
#10560=ORIENTED_EDGE('',*,*,#7348,.F.);
#10561=ORIENTED_EDGE('',*,*,#7349,.T.);
#10562=ORIENTED_EDGE('',*,*,#7350,.T.);
#10563=ORIENTED_EDGE('',*,*,#7351,.F.);
#10564=ORIENTED_EDGE('',*,*,#7352,.F.);
#10565=ORIENTED_EDGE('',*,*,#7353,.T.);
#10566=ORIENTED_EDGE('',*,*,#7354,.T.);
#10567=ORIENTED_EDGE('',*,*,#7355,.F.);
#10568=ORIENTED_EDGE('',*,*,#7356,.F.);
#10569=ORIENTED_EDGE('',*,*,#7357,.T.);
#10570=ORIENTED_EDGE('',*,*,#7358,.T.);
#10571=ORIENTED_EDGE('',*,*,#7359,.F.);
#10572=ORIENTED_EDGE('',*,*,#7360,.F.);
#10573=ORIENTED_EDGE('',*,*,#7361,.T.);
#10574=ORIENTED_EDGE('',*,*,#7362,.T.);
#10575=ORIENTED_EDGE('',*,*,#7363,.F.);
#10576=ORIENTED_EDGE('',*,*,#7364,.T.);
#10577=ORIENTED_EDGE('',*,*,#7365,.T.);
#10578=ORIENTED_EDGE('',*,*,#7366,.F.);
#10579=ORIENTED_EDGE('',*,*,#7367,.T.);
#10580=ORIENTED_EDGE('',*,*,#7368,.F.);
#10581=ORIENTED_EDGE('',*,*,#7369,.T.);
#10582=ORIENTED_EDGE('',*,*,#7370,.T.);
#10583=ORIENTED_EDGE('',*,*,#7371,.T.);
#10584=ORIENTED_EDGE('',*,*,#7372,.T.);
#10585=ORIENTED_EDGE('',*,*,#7373,.T.);
#10586=ORIENTED_EDGE('',*,*,#7374,.F.);
#10587=ORIENTED_EDGE('',*,*,#7375,.T.);
#10588=ORIENTED_EDGE('',*,*,#7376,.T.);
#10589=ORIENTED_EDGE('',*,*,#7377,.T.);
#10590=ORIENTED_EDGE('',*,*,#7378,.F.);
#10591=ORIENTED_EDGE('',*,*,#7379,.T.);
#10592=ORIENTED_EDGE('',*,*,#7366,.T.);
#10593=ORIENTED_EDGE('',*,*,#7380,.T.);
#10594=ORIENTED_EDGE('',*,*,#7368,.T.);
#10595=ORIENTED_EDGE('',*,*,#7381,.T.);
#10596=ORIENTED_EDGE('',*,*,#7374,.T.);
#10597=ORIENTED_EDGE('',*,*,#7382,.T.);
#10598=ORIENTED_EDGE('',*,*,#7378,.T.);
#10599=ORIENTED_EDGE('',*,*,#7383,.T.);
#10600=ORIENTED_EDGE('',*,*,#7384,.F.);
#10601=ORIENTED_EDGE('',*,*,#7350,.F.);
#10602=ORIENTED_EDGE('',*,*,#7385,.F.);
#10603=ORIENTED_EDGE('',*,*,#7386,.F.);
#10604=ORIENTED_EDGE('',*,*,#7387,.F.);
#10605=ORIENTED_EDGE('',*,*,#7354,.F.);
#10606=ORIENTED_EDGE('',*,*,#7388,.F.);
#10607=ORIENTED_EDGE('',*,*,#7389,.F.);
#10608=ORIENTED_EDGE('',*,*,#7390,.F.);
#10609=ORIENTED_EDGE('',*,*,#7358,.F.);
#10610=ORIENTED_EDGE('',*,*,#7391,.F.);
#10611=ORIENTED_EDGE('',*,*,#7392,.F.);
#10612=ORIENTED_EDGE('',*,*,#7393,.F.);
#10613=ORIENTED_EDGE('',*,*,#7362,.F.);
#10614=ORIENTED_EDGE('',*,*,#7394,.F.);
#10615=ORIENTED_EDGE('',*,*,#7395,.F.);
#10616=ORIENTED_EDGE('',*,*,#7370,.F.);
#10617=ORIENTED_EDGE('',*,*,#7396,.T.);
#10618=ORIENTED_EDGE('',*,*,#7364,.F.);
#10619=ORIENTED_EDGE('',*,*,#7397,.T.);
#10620=ORIENTED_EDGE('',*,*,#7376,.F.);
#10621=ORIENTED_EDGE('',*,*,#7398,.T.);
#10622=ORIENTED_EDGE('',*,*,#7372,.F.);
#10623=ORIENTED_EDGE('',*,*,#7399,.T.);
#10624=ORIENTED_EDGE('',*,*,#7348,.T.);
#10625=ORIENTED_EDGE('',*,*,#7400,.T.);
#10626=ORIENTED_EDGE('',*,*,#7401,.T.);
#10627=ORIENTED_EDGE('',*,*,#7402,.T.);
#10628=ORIENTED_EDGE('',*,*,#7352,.T.);
#10629=ORIENTED_EDGE('',*,*,#7403,.T.);
#10630=ORIENTED_EDGE('',*,*,#7404,.T.);
#10631=ORIENTED_EDGE('',*,*,#7405,.T.);
#10632=ORIENTED_EDGE('',*,*,#7356,.T.);
#10633=ORIENTED_EDGE('',*,*,#7406,.T.);
#10634=ORIENTED_EDGE('',*,*,#7407,.T.);
#10635=ORIENTED_EDGE('',*,*,#7408,.T.);
#10636=ORIENTED_EDGE('',*,*,#7360,.T.);
#10637=ORIENTED_EDGE('',*,*,#7409,.T.);
#10638=ORIENTED_EDGE('',*,*,#7410,.T.);
#10639=ORIENTED_EDGE('',*,*,#7411,.T.);
#10640=ORIENTED_EDGE('',*,*,#7394,.T.);
#10641=ORIENTED_EDGE('',*,*,#7361,.F.);
#10642=ORIENTED_EDGE('',*,*,#7411,.F.);
#10643=ORIENTED_EDGE('',*,*,#7412,.T.);
#10644=ORIENTED_EDGE('',*,*,#7395,.T.);
#10645=ORIENTED_EDGE('',*,*,#7412,.F.);
#10646=ORIENTED_EDGE('',*,*,#7410,.F.);
#10647=ORIENTED_EDGE('',*,*,#7413,.T.);
#10648=ORIENTED_EDGE('',*,*,#7393,.T.);
#10649=ORIENTED_EDGE('',*,*,#7413,.F.);
#10650=ORIENTED_EDGE('',*,*,#7409,.F.);
#10651=ORIENTED_EDGE('',*,*,#7363,.T.);
#10652=ORIENTED_EDGE('',*,*,#7391,.T.);
#10653=ORIENTED_EDGE('',*,*,#7357,.F.);
#10654=ORIENTED_EDGE('',*,*,#7408,.F.);
#10655=ORIENTED_EDGE('',*,*,#7414,.T.);
#10656=ORIENTED_EDGE('',*,*,#7392,.T.);
#10657=ORIENTED_EDGE('',*,*,#7414,.F.);
#10658=ORIENTED_EDGE('',*,*,#7407,.F.);
#10659=ORIENTED_EDGE('',*,*,#7415,.T.);
#10660=ORIENTED_EDGE('',*,*,#7390,.T.);
#10661=ORIENTED_EDGE('',*,*,#7415,.F.);
#10662=ORIENTED_EDGE('',*,*,#7406,.F.);
#10663=ORIENTED_EDGE('',*,*,#7359,.T.);
#10664=ORIENTED_EDGE('',*,*,#7388,.T.);
#10665=ORIENTED_EDGE('',*,*,#7353,.F.);
#10666=ORIENTED_EDGE('',*,*,#7405,.F.);
#10667=ORIENTED_EDGE('',*,*,#7416,.T.);
#10668=ORIENTED_EDGE('',*,*,#7389,.T.);
#10669=ORIENTED_EDGE('',*,*,#7416,.F.);
#10670=ORIENTED_EDGE('',*,*,#7404,.F.);
#10671=ORIENTED_EDGE('',*,*,#7417,.T.);
#10672=ORIENTED_EDGE('',*,*,#7387,.T.);
#10673=ORIENTED_EDGE('',*,*,#7417,.F.);
#10674=ORIENTED_EDGE('',*,*,#7403,.F.);
#10675=ORIENTED_EDGE('',*,*,#7355,.T.);
#10676=ORIENTED_EDGE('',*,*,#7385,.T.);
#10677=ORIENTED_EDGE('',*,*,#7349,.F.);
#10678=ORIENTED_EDGE('',*,*,#7402,.F.);
#10679=ORIENTED_EDGE('',*,*,#7418,.T.);
#10680=ORIENTED_EDGE('',*,*,#7386,.T.);
#10681=ORIENTED_EDGE('',*,*,#7418,.F.);
#10682=ORIENTED_EDGE('',*,*,#7401,.F.);
#10683=ORIENTED_EDGE('',*,*,#7419,.T.);
#10684=ORIENTED_EDGE('',*,*,#7384,.T.);
#10685=ORIENTED_EDGE('',*,*,#7419,.F.);
#10686=ORIENTED_EDGE('',*,*,#7400,.F.);
#10687=ORIENTED_EDGE('',*,*,#7351,.T.);
#10688=ORIENTED_EDGE('',*,*,#7380,.F.);
#10689=ORIENTED_EDGE('',*,*,#7365,.F.);
#10690=ORIENTED_EDGE('',*,*,#7396,.F.);
#10691=ORIENTED_EDGE('',*,*,#7369,.F.);
#10692=ORIENTED_EDGE('',*,*,#7383,.F.);
#10693=ORIENTED_EDGE('',*,*,#7377,.F.);
#10694=ORIENTED_EDGE('',*,*,#7397,.F.);
#10695=ORIENTED_EDGE('',*,*,#7367,.F.);
#10696=ORIENTED_EDGE('',*,*,#7382,.F.);
#10697=ORIENTED_EDGE('',*,*,#7373,.F.);
#10698=ORIENTED_EDGE('',*,*,#7398,.F.);
#10699=ORIENTED_EDGE('',*,*,#7379,.F.);
#10700=ORIENTED_EDGE('',*,*,#7381,.F.);
#10701=ORIENTED_EDGE('',*,*,#7371,.F.);
#10702=ORIENTED_EDGE('',*,*,#7399,.F.);
#10703=ORIENTED_EDGE('',*,*,#7375,.F.);
#10704=ORIENTED_EDGE('',*,*,#7420,.F.);
#10705=ORIENTED_EDGE('',*,*,#7421,.T.);
#10706=ORIENTED_EDGE('',*,*,#7422,.T.);
#10707=ORIENTED_EDGE('',*,*,#7421,.F.);
#10708=ORIENTED_EDGE('',*,*,#7423,.F.);
#10709=ORIENTED_EDGE('',*,*,#7424,.T.);
#10710=ORIENTED_EDGE('',*,*,#7425,.T.);
#10711=ORIENTED_EDGE('',*,*,#7424,.F.);
#10712=ORIENTED_EDGE('',*,*,#7426,.F.);
#10713=ORIENTED_EDGE('',*,*,#7427,.F.);
#10714=ORIENTED_EDGE('',*,*,#7428,.F.);
#10715=ORIENTED_EDGE('',*,*,#7429,.T.);
#10716=ORIENTED_EDGE('',*,*,#7430,.F.);
#10717=ORIENTED_EDGE('',*,*,#7431,.F.);
#10718=ORIENTED_EDGE('',*,*,#7432,.F.);
#10719=ORIENTED_EDGE('',*,*,#7427,.T.);
#10720=ORIENTED_EDGE('',*,*,#7433,.F.);
#10721=ORIENTED_EDGE('',*,*,#7434,.F.);
#10722=ORIENTED_EDGE('',*,*,#7435,.F.);
#10723=ORIENTED_EDGE('',*,*,#7431,.T.);
#10724=ORIENTED_EDGE('',*,*,#7436,.F.);
#10725=ORIENTED_EDGE('',*,*,#7437,.F.);
#10726=ORIENTED_EDGE('',*,*,#7438,.F.);
#10727=ORIENTED_EDGE('',*,*,#7434,.T.);
#10728=ORIENTED_EDGE('',*,*,#7439,.F.);
#10729=ORIENTED_EDGE('',*,*,#7440,.F.);
#10730=ORIENTED_EDGE('',*,*,#7441,.F.);
#10731=ORIENTED_EDGE('',*,*,#7437,.T.);
#10732=ORIENTED_EDGE('',*,*,#7442,.F.);
#10733=ORIENTED_EDGE('',*,*,#7443,.F.);
#10734=ORIENTED_EDGE('',*,*,#7444,.F.);
#10735=ORIENTED_EDGE('',*,*,#7440,.T.);
#10736=ORIENTED_EDGE('',*,*,#7420,.T.);
#10737=ORIENTED_EDGE('',*,*,#7423,.T.);
#10738=ORIENTED_EDGE('',*,*,#7445,.F.);
#10739=ORIENTED_EDGE('',*,*,#7446,.F.);
#10740=ORIENTED_EDGE('',*,*,#7447,.F.);
#10741=ORIENTED_EDGE('',*,*,#7443,.T.);
#10742=ORIENTED_EDGE('',*,*,#7448,.F.);
#10743=ORIENTED_EDGE('',*,*,#7449,.F.);
#10744=ORIENTED_EDGE('',*,*,#7450,.F.);
#10745=ORIENTED_EDGE('',*,*,#7446,.T.);
#10746=ORIENTED_EDGE('',*,*,#7451,.F.);
#10747=ORIENTED_EDGE('',*,*,#7452,.F.);
#10748=ORIENTED_EDGE('',*,*,#7453,.F.);
#10749=ORIENTED_EDGE('',*,*,#7449,.T.);
#10750=ORIENTED_EDGE('',*,*,#7454,.F.);
#10751=ORIENTED_EDGE('',*,*,#7455,.F.);
#10752=ORIENTED_EDGE('',*,*,#7456,.F.);
#10753=ORIENTED_EDGE('',*,*,#7452,.T.);
#10754=ORIENTED_EDGE('',*,*,#7457,.F.);
#10755=ORIENTED_EDGE('',*,*,#7458,.F.);
#10756=ORIENTED_EDGE('',*,*,#7459,.F.);
#10757=ORIENTED_EDGE('',*,*,#7455,.T.);
#10758=ORIENTED_EDGE('',*,*,#7460,.F.);
#10759=ORIENTED_EDGE('',*,*,#7429,.F.);
#10760=ORIENTED_EDGE('',*,*,#7461,.F.);
#10761=ORIENTED_EDGE('',*,*,#7458,.T.);
#10762=ORIENTED_EDGE('',*,*,#7422,.F.);
#10763=ORIENTED_EDGE('',*,*,#7425,.F.);
#10764=ORIENTED_EDGE('',*,*,#7461,.T.);
#10765=ORIENTED_EDGE('',*,*,#7428,.T.);
#10766=ORIENTED_EDGE('',*,*,#7432,.T.);
#10767=ORIENTED_EDGE('',*,*,#7435,.T.);
#10768=ORIENTED_EDGE('',*,*,#7438,.T.);
#10769=ORIENTED_EDGE('',*,*,#7441,.T.);
#10770=ORIENTED_EDGE('',*,*,#7444,.T.);
#10771=ORIENTED_EDGE('',*,*,#7447,.T.);
#10772=ORIENTED_EDGE('',*,*,#7450,.T.);
#10773=ORIENTED_EDGE('',*,*,#7453,.T.);
#10774=ORIENTED_EDGE('',*,*,#7456,.T.);
#10775=ORIENTED_EDGE('',*,*,#7459,.T.);
#10776=ORIENTED_EDGE('',*,*,#7430,.T.);
#10777=ORIENTED_EDGE('',*,*,#7426,.T.);
#10778=ORIENTED_EDGE('',*,*,#7460,.T.);
#10779=ORIENTED_EDGE('',*,*,#7457,.T.);
#10780=ORIENTED_EDGE('',*,*,#7454,.T.);
#10781=ORIENTED_EDGE('',*,*,#7451,.T.);
#10782=ORIENTED_EDGE('',*,*,#7448,.T.);
#10783=ORIENTED_EDGE('',*,*,#7445,.T.);
#10784=ORIENTED_EDGE('',*,*,#7442,.T.);
#10785=ORIENTED_EDGE('',*,*,#7439,.T.);
#10786=ORIENTED_EDGE('',*,*,#7436,.T.);
#10787=ORIENTED_EDGE('',*,*,#7433,.T.);
#10788=ORIENTED_EDGE('',*,*,#7462,.F.);
#10789=ORIENTED_EDGE('',*,*,#7463,.T.);
#10790=ORIENTED_EDGE('',*,*,#7464,.T.);
#10791=ORIENTED_EDGE('',*,*,#7463,.F.);
#10792=ORIENTED_EDGE('',*,*,#7465,.F.);
#10793=ORIENTED_EDGE('',*,*,#7466,.T.);
#10794=ORIENTED_EDGE('',*,*,#7467,.T.);
#10795=ORIENTED_EDGE('',*,*,#7466,.F.);
#10796=ORIENTED_EDGE('',*,*,#7468,.T.);
#10797=ORIENTED_EDGE('',*,*,#7469,.F.);
#10798=ORIENTED_EDGE('',*,*,#7470,.F.);
#10799=ORIENTED_EDGE('',*,*,#7471,.T.);
#10800=ORIENTED_EDGE('',*,*,#7464,.F.);
#10801=ORIENTED_EDGE('',*,*,#7467,.F.);
#10802=ORIENTED_EDGE('',*,*,#7472,.T.);
#10803=ORIENTED_EDGE('',*,*,#7473,.F.);
#10804=ORIENTED_EDGE('',*,*,#7474,.F.);
#10805=ORIENTED_EDGE('',*,*,#7469,.T.);
#10806=ORIENTED_EDGE('',*,*,#7475,.T.);
#10807=ORIENTED_EDGE('',*,*,#7476,.F.);
#10808=ORIENTED_EDGE('',*,*,#7477,.F.);
#10809=ORIENTED_EDGE('',*,*,#7473,.T.);
#10810=ORIENTED_EDGE('',*,*,#7478,.T.);
#10811=ORIENTED_EDGE('',*,*,#7479,.F.);
#10812=ORIENTED_EDGE('',*,*,#7480,.F.);
#10813=ORIENTED_EDGE('',*,*,#7476,.T.);
#10814=ORIENTED_EDGE('',*,*,#7462,.T.);
#10815=ORIENTED_EDGE('',*,*,#7465,.T.);
#10816=ORIENTED_EDGE('',*,*,#7481,.T.);
#10817=ORIENTED_EDGE('',*,*,#7482,.F.);
#10818=ORIENTED_EDGE('',*,*,#7483,.F.);
#10819=ORIENTED_EDGE('',*,*,#7479,.T.);
#10820=ORIENTED_EDGE('',*,*,#7484,.T.);
#10821=ORIENTED_EDGE('',*,*,#7485,.F.);
#10822=ORIENTED_EDGE('',*,*,#7486,.F.);
#10823=ORIENTED_EDGE('',*,*,#7482,.T.);
#10824=ORIENTED_EDGE('',*,*,#7487,.T.);
#10825=ORIENTED_EDGE('',*,*,#7488,.F.);
#10826=ORIENTED_EDGE('',*,*,#7489,.F.);
#10827=ORIENTED_EDGE('',*,*,#7485,.T.);
#10828=ORIENTED_EDGE('',*,*,#7490,.T.);
#10829=ORIENTED_EDGE('',*,*,#7491,.F.);
#10830=ORIENTED_EDGE('',*,*,#7492,.F.);
#10831=ORIENTED_EDGE('',*,*,#7488,.T.);
#10832=ORIENTED_EDGE('',*,*,#7493,.T.);
#10833=ORIENTED_EDGE('',*,*,#7471,.F.);
#10834=ORIENTED_EDGE('',*,*,#7494,.F.);
#10835=ORIENTED_EDGE('',*,*,#7491,.T.);
#10836=ORIENTED_EDGE('',*,*,#7470,.T.);
#10837=ORIENTED_EDGE('',*,*,#7474,.T.);
#10838=ORIENTED_EDGE('',*,*,#7477,.T.);
#10839=ORIENTED_EDGE('',*,*,#7480,.T.);
#10840=ORIENTED_EDGE('',*,*,#7483,.T.);
#10841=ORIENTED_EDGE('',*,*,#7486,.T.);
#10842=ORIENTED_EDGE('',*,*,#7489,.T.);
#10843=ORIENTED_EDGE('',*,*,#7492,.T.);
#10844=ORIENTED_EDGE('',*,*,#7494,.T.);
#10845=ORIENTED_EDGE('',*,*,#7468,.F.);
#10846=ORIENTED_EDGE('',*,*,#7493,.F.);
#10847=ORIENTED_EDGE('',*,*,#7490,.F.);
#10848=ORIENTED_EDGE('',*,*,#7487,.F.);
#10849=ORIENTED_EDGE('',*,*,#7484,.F.);
#10850=ORIENTED_EDGE('',*,*,#7481,.F.);
#10851=ORIENTED_EDGE('',*,*,#7478,.F.);
#10852=ORIENTED_EDGE('',*,*,#7475,.F.);
#10853=ORIENTED_EDGE('',*,*,#7472,.F.);
#10854=ORIENTED_EDGE('',*,*,#7495,.F.);
#10855=ORIENTED_EDGE('',*,*,#7496,.T.);
#10856=ORIENTED_EDGE('',*,*,#7497,.T.);
#10857=ORIENTED_EDGE('',*,*,#7496,.F.);
#10858=ORIENTED_EDGE('',*,*,#7498,.F.);
#10859=ORIENTED_EDGE('',*,*,#7499,.T.);
#10860=ORIENTED_EDGE('',*,*,#7500,.T.);
#10861=ORIENTED_EDGE('',*,*,#7499,.F.);
#10862=ORIENTED_EDGE('',*,*,#7501,.F.);
#10863=ORIENTED_EDGE('',*,*,#7502,.F.);
#10864=ORIENTED_EDGE('',*,*,#7503,.T.);
#10865=ORIENTED_EDGE('',*,*,#7504,.T.);
#10866=ORIENTED_EDGE('',*,*,#7497,.F.);
#10867=ORIENTED_EDGE('',*,*,#7500,.F.);
#10868=ORIENTED_EDGE('',*,*,#7505,.F.);
#10869=ORIENTED_EDGE('',*,*,#7504,.F.);
#10870=ORIENTED_EDGE('',*,*,#7506,.T.);
#10871=ORIENTED_EDGE('',*,*,#7507,.T.);
#10872=ORIENTED_EDGE('',*,*,#7508,.F.);
#10873=ORIENTED_EDGE('',*,*,#7507,.F.);
#10874=ORIENTED_EDGE('',*,*,#7509,.T.);
#10875=ORIENTED_EDGE('',*,*,#7510,.T.);
#10876=ORIENTED_EDGE('',*,*,#7511,.F.);
#10877=ORIENTED_EDGE('',*,*,#7510,.F.);
#10878=ORIENTED_EDGE('',*,*,#7512,.T.);
#10879=ORIENTED_EDGE('',*,*,#7513,.T.);
#10880=ORIENTED_EDGE('',*,*,#7495,.T.);
#10881=ORIENTED_EDGE('',*,*,#7498,.T.);
#10882=ORIENTED_EDGE('',*,*,#7514,.F.);
#10883=ORIENTED_EDGE('',*,*,#7513,.F.);
#10884=ORIENTED_EDGE('',*,*,#7515,.T.);
#10885=ORIENTED_EDGE('',*,*,#7516,.T.);
#10886=ORIENTED_EDGE('',*,*,#7517,.F.);
#10887=ORIENTED_EDGE('',*,*,#7516,.F.);
#10888=ORIENTED_EDGE('',*,*,#7518,.T.);
#10889=ORIENTED_EDGE('',*,*,#7519,.T.);
#10890=ORIENTED_EDGE('',*,*,#7520,.F.);
#10891=ORIENTED_EDGE('',*,*,#7519,.F.);
#10892=ORIENTED_EDGE('',*,*,#7521,.T.);
#10893=ORIENTED_EDGE('',*,*,#7522,.T.);
#10894=ORIENTED_EDGE('',*,*,#7523,.F.);
#10895=ORIENTED_EDGE('',*,*,#7522,.F.);
#10896=ORIENTED_EDGE('',*,*,#7524,.T.);
#10897=ORIENTED_EDGE('',*,*,#7525,.T.);
#10898=ORIENTED_EDGE('',*,*,#7526,.F.);
#10899=ORIENTED_EDGE('',*,*,#7525,.F.);
#10900=ORIENTED_EDGE('',*,*,#7527,.T.);
#10901=ORIENTED_EDGE('',*,*,#7502,.T.);
#10902=ORIENTED_EDGE('',*,*,#7503,.F.);
#10903=ORIENTED_EDGE('',*,*,#7527,.F.);
#10904=ORIENTED_EDGE('',*,*,#7524,.F.);
#10905=ORIENTED_EDGE('',*,*,#7521,.F.);
#10906=ORIENTED_EDGE('',*,*,#7518,.F.);
#10907=ORIENTED_EDGE('',*,*,#7515,.F.);
#10908=ORIENTED_EDGE('',*,*,#7512,.F.);
#10909=ORIENTED_EDGE('',*,*,#7509,.F.);
#10910=ORIENTED_EDGE('',*,*,#7506,.F.);
#10911=ORIENTED_EDGE('',*,*,#7501,.T.);
#10912=ORIENTED_EDGE('',*,*,#7505,.T.);
#10913=ORIENTED_EDGE('',*,*,#7508,.T.);
#10914=ORIENTED_EDGE('',*,*,#7511,.T.);
#10915=ORIENTED_EDGE('',*,*,#7514,.T.);
#10916=ORIENTED_EDGE('',*,*,#7517,.T.);
#10917=ORIENTED_EDGE('',*,*,#7520,.T.);
#10918=ORIENTED_EDGE('',*,*,#7523,.T.);
#10919=ORIENTED_EDGE('',*,*,#7526,.T.);
#10920=CYLINDRICAL_SURFACE('',#11897,160.);
#10921=CYLINDRICAL_SURFACE('',#11904,2.5);
#10922=CYLINDRICAL_SURFACE('',#11907,2.5);
#10923=CYLINDRICAL_SURFACE('',#11911,2.5);
#10924=CYLINDRICAL_SURFACE('',#11943,4.49999999999998);
#10925=CYLINDRICAL_SURFACE('',#11948,4.49999999999998);
#10926=CYLINDRICAL_SURFACE('',#11953,4.49999999999998);
#10927=CYLINDRICAL_SURFACE('',#11958,4.49999999999998);
#10928=CYLINDRICAL_SURFACE('',#11963,4.49999999999998);
#10929=CYLINDRICAL_SURFACE('',#11968,4.49999999999998);
#10930=CYLINDRICAL_SURFACE('',#11970,195.);
#10931=CYLINDRICAL_SURFACE('',#11978,35.5);
#10932=CYLINDRICAL_SURFACE('',#11979,4.5);
#10933=CYLINDRICAL_SURFACE('',#11982,4.5);
#10934=CYLINDRICAL_SURFACE('',#11985,4.5);
#10935=CYLINDRICAL_SURFACE('',#11988,4.5);
#10936=CYLINDRICAL_SURFACE('',#11991,25.);
#10937=CYLINDRICAL_SURFACE('',#11994,160.);
#10938=CYLINDRICAL_SURFACE('',#11998,15.);
#10939=CYLINDRICAL_SURFACE('',#12003,170.);
#10940=CYLINDRICAL_SURFACE('',#12031,175.);
#10941=CYLINDRICAL_SURFACE('',#12039,285.);
#10942=CYLINDRICAL_SURFACE('',#12066,100.);
#10943=CYLINDRICAL_SURFACE('',#12069,100.);
#10944=CYLINDRICAL_SURFACE('',#12074,100.);
#10945=CYLINDRICAL_SURFACE('',#12077,35.);
#10946=CYLINDRICAL_SURFACE('',#12084,35.);
#10947=CYLINDRICAL_SURFACE('',#12091,35.);
#10948=CYLINDRICAL_SURFACE('',#12097,35.);
#10949=CYLINDRICAL_SURFACE('',#12111,185.);
#10950=CYLINDRICAL_SURFACE('',#12119,275.);
#10951=CYLINDRICAL_SURFACE('',#12137,110.);
#10952=CYLINDRICAL_SURFACE('',#12140,110.);
#10953=CYLINDRICAL_SURFACE('',#12145,110.);
#10954=CYLINDRICAL_SURFACE('',#12148,25.);
#10955=CYLINDRICAL_SURFACE('',#12155,25.);
#10956=CYLINDRICAL_SURFACE('',#12162,25.);
#10957=CYLINDRICAL_SURFACE('',#12168,25.);
#10958=CYLINDRICAL_SURFACE('',#12217,2.5);
#10959=CYLINDRICAL_SURFACE('',#12219,2.5);
#10960=CYLINDRICAL_SURFACE('',#12234,2.5);
#10961=CYLINDRICAL_SURFACE('',#12236,2.5);
#10962=CYLINDRICAL_SURFACE('',#12237,2.5);
#10963=CYLINDRICAL_SURFACE('',#12239,2.50000000000001);
#10964=CYLINDRICAL_SURFACE('',#12241,2.5);
#10965=CYLINDRICAL_SURFACE('',#12243,2.5);
#10966=CYLINDRICAL_SURFACE('',#12245,2.50000000000001);
#10967=CYLINDRICAL_SURFACE('',#12247,2.5);
#10968=CYLINDRICAL_SURFACE('',#12249,2.5);
#10969=CYLINDRICAL_SURFACE('',#12251,2.5);
#10970=CYLINDRICAL_SURFACE('',#12266,2.5);
#10971=CYLINDRICAL_SURFACE('',#12267,2.5);
#10972=CYLINDRICAL_SURFACE('',#12269,2.5);
#10973=CYLINDRICAL_SURFACE('',#12271,2.5);
#10974=CYLINDRICAL_SURFACE('',#12273,2.5);
#10975=CYLINDRICAL_SURFACE('',#12281,2.5);
#10976=CYLINDRICAL_SURFACE('',#12283,2.5);
#10977=CYLINDRICAL_SURFACE('',#12284,2.5);
#10978=CYLINDRICAL_SURFACE('',#12286,2.5);
#10979=CYLINDRICAL_SURFACE('',#12288,2.5);
#10980=CYLINDRICAL_SURFACE('',#12290,2.5);
#10981=CYLINDRICAL_SURFACE('',#12299,2.5);
#10982=CYLINDRICAL_SURFACE('',#12300,2.5);
#10983=CYLINDRICAL_SURFACE('',#12302,2.5);
#10984=CYLINDRICAL_SURFACE('',#12310,2.5);
#10985=CYLINDRICAL_SURFACE('',#12311,2.5);
#10986=CYLINDRICAL_SURFACE('',#12312,2.5);
#10987=CYLINDRICAL_SURFACE('',#12313,2.5);
#10988=CYLINDRICAL_SURFACE('',#12321,2.50000000000001);
#10989=CYLINDRICAL_SURFACE('',#12324,2.5);
#10990=CYLINDRICAL_SURFACE('',#12326,2.5);
#10991=CYLINDRICAL_SURFACE('',#12328,2.50000000000001);
#10992=CYLINDRICAL_SURFACE('',#12330,2.5);
#10993=CYLINDRICAL_SURFACE('',#12342,2.5);
#10994=CYLINDRICAL_SURFACE('',#12343,2.5);
#10995=CYLINDRICAL_SURFACE('',#12345,2.5);
#10996=CYLINDRICAL_SURFACE('',#12347,2.5);
#10997=CYLINDRICAL_SURFACE('',#12349,2.5);
#10998=CYLINDRICAL_SURFACE('',#12359,2.5);
#10999=CYLINDRICAL_SURFACE('',#12361,2.5);
#11000=CYLINDRICAL_SURFACE('',#12363,2.5);
#11001=CYLINDRICAL_SURFACE('',#12364,2.5);
#11002=CYLINDRICAL_SURFACE('',#12374,2.5);
#11003=CYLINDRICAL_SURFACE('',#12376,2.5);
#11004=CYLINDRICAL_SURFACE('',#12378,2.5);
#11005=CYLINDRICAL_SURFACE('',#12384,2.5);
#11006=CYLINDRICAL_SURFACE('',#12386,2.5);
#11007=CYLINDRICAL_SURFACE('',#12388,2.5);
#11008=CYLINDRICAL_SURFACE('',#12390,2.5);
#11009=CYLINDRICAL_SURFACE('',#12403,2.5);
#11010=CYLINDRICAL_SURFACE('',#12405,2.5);
#11011=CYLINDRICAL_SURFACE('',#12407,2.5);
#11012=CYLINDRICAL_SURFACE('',#12415,2.5);
#11013=CYLINDRICAL_SURFACE('',#12417,2.5);
#11014=CYLINDRICAL_SURFACE('',#12418,2.5);
#11015=CYLINDRICAL_SURFACE('',#12437,9.5);
#11016=CYLINDRICAL_SURFACE('',#12440,120.);
#11017=CYLINDRICAL_SURFACE('',#12463,160.);
#11018=CYLINDRICAL_SURFACE('',#12488,35.);
#11019=CYLINDRICAL_SURFACE('',#12489,30.);
#11020=CYLINDRICAL_SURFACE('',#12518,156.);
#11021=CYLINDRICAL_SURFACE('',#12523,10.);
#11022=CYLINDRICAL_SURFACE('',#12527,156.);
#11023=CYLINDRICAL_SURFACE('',#12535,156.);
#11024=CYLINDRICAL_SURFACE('',#12543,156.);
#11025=CYLINDRICAL_SURFACE('',#12551,156.);
#11026=CYLINDRICAL_SURFACE('',#12559,156.);
#11027=CYLINDRICAL_SURFACE('',#12567,156.);
#11028=CYLINDRICAL_SURFACE('',#12575,156.);
#11029=CYLINDRICAL_SURFACE('',#12583,156.);
#11030=CYLINDRICAL_SURFACE('',#12591,156.);
#11031=CYLINDRICAL_SURFACE('',#12596,10.);
#11032=CYLINDRICAL_SURFACE('',#12597,9.99999999999999);
#11033=CYLINDRICAL_SURFACE('',#12598,10.);
#11034=CYLINDRICAL_SURFACE('',#12599,10.);
#11035=CYLINDRICAL_SURFACE('',#12600,10.);
#11036=CYLINDRICAL_SURFACE('',#12601,10.);
#11037=CYLINDRICAL_SURFACE('',#12602,10.);
#11038=CYLINDRICAL_SURFACE('',#12603,10.);
#11039=CYLINDRICAL_SURFACE('',#12604,10.);
#11040=CYLINDRICAL_SURFACE('',#12633,5.50000000000001);
#11041=CYLINDRICAL_SURFACE('',#12638,5.50000000000001);
#11042=CYLINDRICAL_SURFACE('',#12643,5.49999999999999);
#11043=CYLINDRICAL_SURFACE('',#12648,5.50000000000001);
#11044=CYLINDRICAL_SURFACE('',#12653,5.49999999999998);
#11045=CYLINDRICAL_SURFACE('',#12658,5.49999999999999);
#11046=CYLINDRICAL_SURFACE('',#12660,145.);
#11047=CYLINDRICAL_SURFACE('',#12663,195.);
#11048=CYLINDRICAL_SURFACE('',#12669,2.54);
#11049=CYLINDRICAL_SURFACE('',#12673,6.85800000000002);
#11050=CYLINDRICAL_SURFACE('',#12677,6.85800000000002);
#11051=CYLINDRICAL_SURFACE('',#12681,2.54);
#11052=CYLINDRICAL_SURFACE('',#12697,2.53999999999999);
#11053=CYLINDRICAL_SURFACE('',#12700,6.85800000000003);
#11054=CYLINDRICAL_SURFACE('',#12703,6.85800000000003);
#11055=CYLINDRICAL_SURFACE('',#12706,2.53999999999999);
#11056=CYLINDRICAL_SURFACE('',#12719,2.53999999999998);
#11057=CYLINDRICAL_SURFACE('',#12722,6.85800000000001);
#11058=CYLINDRICAL_SURFACE('',#12725,6.858);
#11059=CYLINDRICAL_SURFACE('',#12728,2.53999999999998);
#11060=CYLINDRICAL_SURFACE('',#12735,2.53999999999999);
#11061=CYLINDRICAL_SURFACE('',#12739,6.858);
#11062=CYLINDRICAL_SURFACE('',#12743,6.85800000000002);
#11063=CYLINDRICAL_SURFACE('',#12747,2.53999999999999);
#11064=CYLINDRICAL_SURFACE('',#12757,2.53999999999999);
#11065=CYLINDRICAL_SURFACE('',#12761,6.85799999999992);
#11066=CYLINDRICAL_SURFACE('',#12765,6.85799999999992);
#11067=CYLINDRICAL_SURFACE('',#12769,2.53999999999999);
#11068=CYLINDRICAL_SURFACE('',#12785,2.53999999999999);
#11069=CYLINDRICAL_SURFACE('',#12788,6.85800000000003);
#11070=CYLINDRICAL_SURFACE('',#12791,6.85800000000003);
#11071=CYLINDRICAL_SURFACE('',#12794,2.53999999999999);
#11072=CYLINDRICAL_SURFACE('',#12801,2.53999999999999);
#11073=CYLINDRICAL_SURFACE('',#12805,6.85800000000003);
#11074=CYLINDRICAL_SURFACE('',#12809,6.85800000000003);
#11075=CYLINDRICAL_SURFACE('',#12813,2.53999999999999);
#11076=CYLINDRICAL_SURFACE('',#12829,2.53999999999998);
#11077=CYLINDRICAL_SURFACE('',#12832,6.85800000000003);
#11078=CYLINDRICAL_SURFACE('',#12835,6.85800000000003);
#11079=CYLINDRICAL_SURFACE('',#12838,2.53999999999998);
#11080=CYLINDRICAL_SURFACE('',#12851,2.53999999999999);
#11081=CYLINDRICAL_SURFACE('',#12854,6.858);
#11082=CYLINDRICAL_SURFACE('',#12857,6.85800000000003);
#11083=CYLINDRICAL_SURFACE('',#12860,2.53999999999999);
#11084=CYLINDRICAL_SURFACE('',#12873,2.53999999999999);
#11085=CYLINDRICAL_SURFACE('',#12876,6.858);
#11086=CYLINDRICAL_SURFACE('',#12879,6.85800000000003);
#11087=CYLINDRICAL_SURFACE('',#12882,2.53999999999999);
#11088=CYLINDRICAL_SURFACE('',#12889,3.16991999999999);
#11089=CYLINDRICAL_SURFACE('',#12893,4.7625);
#11090=CYLINDRICAL_SURFACE('',#12897,3.16991999999999);
#11091=CYLINDRICAL_SURFACE('',#12906,3.16991999999999);
#11092=CYLINDRICAL_SURFACE('',#12910,4.7625);
#11093=CYLINDRICAL_SURFACE('',#12914,3.16991999999999);
#11094=CYLINDRICAL_SURFACE('',#12923,3.16991999999999);
#11095=CYLINDRICAL_SURFACE('',#12927,4.7625);
#11096=CYLINDRICAL_SURFACE('',#12931,3.16991999999999);
#11097=CYLINDRICAL_SURFACE('',#12940,3.16991999999999);
#11098=CYLINDRICAL_SURFACE('',#12944,4.7625);
#11099=CYLINDRICAL_SURFACE('',#12948,3.16991999999999);
#11100=CYLINDRICAL_SURFACE('',#12961,3.16991999999998);
#11101=CYLINDRICAL_SURFACE('',#12964,4.7625);
#11102=CYLINDRICAL_SURFACE('',#12967,3.16991999999999);
#11103=CYLINDRICAL_SURFACE('',#12974,3.16991999999999);
#11104=CYLINDRICAL_SURFACE('',#12978,4.7625);
#11105=CYLINDRICAL_SURFACE('',#12982,3.16991999999999);
#11106=CYLINDRICAL_SURFACE('',#12995,3.16991999999996);
#11107=CYLINDRICAL_SURFACE('',#12998,4.7625);
#11108=CYLINDRICAL_SURFACE('',#13001,3.16991999999999);
#11109=CYLINDRICAL_SURFACE('',#13012,3.16991999999996);
#11110=CYLINDRICAL_SURFACE('',#13015,4.7625);
#11111=CYLINDRICAL_SURFACE('',#13018,3.16991999999999);
#11112=CYLINDRICAL_SURFACE('',#13025,3.16992000000005);
#11113=CYLINDRICAL_SURFACE('',#13029,4.7625);
#11114=CYLINDRICAL_SURFACE('',#13033,3.16991999999994);
#11115=CYLINDRICAL_SURFACE('',#13046,3.16991999999994);
#11116=CYLINDRICAL_SURFACE('',#13049,4.7625);
#11117=CYLINDRICAL_SURFACE('',#13052,3.16992000000005);
#11118=CYLINDRICAL_SURFACE('',#13057,4.50000000000006);
#11119=CYLINDRICAL_SURFACE('',#13060,4.49999999999995);
#11120=CYLINDRICAL_SURFACE('',#13063,4.49999999999995);
#11121=CYLINDRICAL_SURFACE('',#13066,4.49999999999995);
#11122=CYLINDRICAL_SURFACE('',#13084,4.49999999999995);
#11123=CYLINDRICAL_SURFACE('',#13087,4.49999999999995);
#11124=CYLINDRICAL_SURFACE('',#13090,4.49999999999995);
#11125=CYLINDRICAL_SURFACE('',#13093,4.50000000000006);
#11126=CYLINDRICAL_SURFACE('',#13099,8.74999999999998);
#11127=CYLINDRICAL_SURFACE('',#13102,8.74999999999998);
#11128=CYLINDRICAL_SURFACE('',#13107,2.53999999999999);
#11129=CYLINDRICAL_SURFACE('',#13111,6.85800000000003);
#11130=CYLINDRICAL_SURFACE('',#13115,6.85799999999998);
#11131=CYLINDRICAL_SURFACE('',#13119,2.53999999999999);
#11132=CYLINDRICAL_SURFACE('',#13127,4.5);
#11133=CYLINDRICAL_SURFACE('',#13130,4.5);
#11134=CYLINDRICAL_SURFACE('',#13135,3.16991999999999);
#11135=CYLINDRICAL_SURFACE('',#13139,4.7625);
#11136=CYLINDRICAL_SURFACE('',#13143,3.16991999999999);
#11137=CYLINDRICAL_SURFACE('',#13150,4.5);
#11138=CYLINDRICAL_SURFACE('',#13153,4.5);
#11139=CYLINDRICAL_SURFACE('',#13158,3.16991999999999);
#11140=CYLINDRICAL_SURFACE('',#13162,4.7625);
#11141=CYLINDRICAL_SURFACE('',#13166,3.16991999999999);
#11142=ADVANCED_FACE('',(#703),#10920,.F.);
#11143=ADVANCED_FACE('',(#704),#658,.T.);
#11144=ADVANCED_FACE('',(#705),#10921,.F.);
#11145=ADVANCED_FACE('',(#706),#10922,.F.);
#11146=ADVANCED_FACE('',(#707),#10923,.F.);
#11147=ADVANCED_FACE('',(#708),#634,.F.);
#11148=ADVANCED_FACE('',(#709),#635,.F.);
#11149=ADVANCED_FACE('',(#710),#636,.F.);
#11150=ADVANCED_FACE('',(#711),#637,.F.);
#11151=ADVANCED_FACE('',(#712),#659,.T.);
#11152=ADVANCED_FACE('',(#713),#660,.T.);
#11153=ADVANCED_FACE('',(#714),#617,.F.);
#11154=ADVANCED_FACE('',(#715),#10924,.F.);
#11155=ADVANCED_FACE('',(#716),#618,.F.);
#11156=ADVANCED_FACE('',(#717),#10925,.F.);
#11157=ADVANCED_FACE('',(#718),#619,.F.);
#11158=ADVANCED_FACE('',(#719),#10926,.F.);
#11159=ADVANCED_FACE('',(#720),#620,.F.);
#11160=ADVANCED_FACE('',(#721),#10927,.F.);
#11161=ADVANCED_FACE('',(#722),#621,.F.);
#11162=ADVANCED_FACE('',(#723),#10928,.F.);
#11163=ADVANCED_FACE('',(#724),#622,.F.);
#11164=ADVANCED_FACE('',(#725),#10929,.F.);
#11165=ADVANCED_FACE('',(#726),#10930,.T.);
#11166=ADVANCED_FACE('',(#727),#623,.F.);
#11167=ADVANCED_FACE('',(#728),#624,.F.);
#11168=ADVANCED_FACE('',(#729),#10931,.F.);
#11169=ADVANCED_FACE('',(#730),#10932,.F.);
#11170=ADVANCED_FACE('',(#731),#10933,.F.);
#11171=ADVANCED_FACE('',(#732),#10934,.F.);
#11172=ADVANCED_FACE('',(#733),#10935,.F.);
#11173=ADVANCED_FACE('',(#734),#10936,.T.);
#11174=ADVANCED_FACE('',(#735),#10937,.F.);
#11175=ADVANCED_FACE('',(#736),#10938,.F.);
#11176=ADVANCED_FACE('',(#737,#542,#543),#10939,.T.);
#11177=ADVANCED_FACE('',(#738,#544,#545),#205,.F.);
#11178=ADVANCED_FACE('',(#739,#546,#547),#206,.F.);
#11179=ADVANCED_FACE('',(#740,#548,#549),#207,.T.);
#11180=ADVANCED_FACE('',(#741,#550),#208,.F.);
#11181=ADVANCED_FACE('',(#742),#10940,.F.);
#11182=ADVANCED_FACE('',(#743),#209,.F.);
#11183=ADVANCED_FACE('',(#744),#10941,.T.);
#11184=ADVANCED_FACE('',(#745),#210,.F.);
#11185=ADVANCED_FACE('',(#746,#551),#211,.T.);
#11186=ADVANCED_FACE('',(#747),#212,.F.);
#11187=ADVANCED_FACE('',(#748),#213,.F.);
#11188=ADVANCED_FACE('',(#749),#214,.F.);
#11189=ADVANCED_FACE('',(#750),#215,.F.);
#11190=ADVANCED_FACE('',(#751),#10942,.F.);
#11191=ADVANCED_FACE('',(#752),#10943,.F.);
#11192=ADVANCED_FACE('',(#753),#10944,.F.);
#11193=ADVANCED_FACE('',(#754),#10945,.T.);
#11194=ADVANCED_FACE('',(#755),#89,.T.);
#11195=ADVANCED_FACE('',(#756),#90,.T.);
#11196=ADVANCED_FACE('',(#757),#661,.T.);
#11197=ADVANCED_FACE('',(#758),#662,.T.);
#11198=ADVANCED_FACE('',(#759),#10946,.T.);
#11199=ADVANCED_FACE('',(#760),#91,.T.);
#11200=ADVANCED_FACE('',(#761),#92,.T.);
#11201=ADVANCED_FACE('',(#762),#663,.T.);
#11202=ADVANCED_FACE('',(#763),#664,.T.);
#11203=ADVANCED_FACE('',(#764),#10947,.T.);
#11204=ADVANCED_FACE('',(#765),#665,.T.);
#11205=ADVANCED_FACE('',(#766),#93,.T.);
#11206=ADVANCED_FACE('',(#767),#666,.T.);
#11207=ADVANCED_FACE('',(#768),#10948,.T.);
#11208=ADVANCED_FACE('',(#769),#667,.T.);
#11209=ADVANCED_FACE('',(#770),#94,.T.);
#11210=ADVANCED_FACE('',(#771),#668,.T.);
#11211=ADVANCED_FACE('',(#772),#95,.F.);
#11212=ADVANCED_FACE('',(#773),#669,.F.);
#11213=ADVANCED_FACE('',(#774),#96,.F.);
#11214=ADVANCED_FACE('',(#775),#97,.F.);
#11215=ADVANCED_FACE('',(#776),#670,.F.);
#11216=ADVANCED_FACE('',(#777),#98,.F.);
#11217=ADVANCED_FACE('',(#778,#552),#216,.T.);
#11218=ADVANCED_FACE('',(#779),#10949,.T.);
#11219=ADVANCED_FACE('',(#780),#217,.T.);
#11220=ADVANCED_FACE('',(#781),#10950,.F.);
#11221=ADVANCED_FACE('',(#782),#218,.T.);
#11222=ADVANCED_FACE('',(#783),#219,.T.);
#11223=ADVANCED_FACE('',(#784),#220,.T.);
#11224=ADVANCED_FACE('',(#785),#221,.T.);
#11225=ADVANCED_FACE('',(#786),#222,.T.);
#11226=ADVANCED_FACE('',(#787),#10951,.T.);
#11227=ADVANCED_FACE('',(#788),#10952,.T.);
#11228=ADVANCED_FACE('',(#789),#10953,.T.);
#11229=ADVANCED_FACE('',(#790),#10954,.F.);
#11230=ADVANCED_FACE('',(#791),#99,.F.);
#11231=ADVANCED_FACE('',(#792),#100,.F.);
#11232=ADVANCED_FACE('',(#793),#671,.F.);
#11233=ADVANCED_FACE('',(#794),#672,.F.);
#11234=ADVANCED_FACE('',(#795),#10955,.F.);
#11235=ADVANCED_FACE('',(#796),#101,.F.);
#11236=ADVANCED_FACE('',(#797),#102,.F.);
#11237=ADVANCED_FACE('',(#798),#673,.F.);
#11238=ADVANCED_FACE('',(#799),#674,.F.);
#11239=ADVANCED_FACE('',(#800),#10956,.F.);
#11240=ADVANCED_FACE('',(#801),#675,.F.);
#11241=ADVANCED_FACE('',(#802),#103,.F.);
#11242=ADVANCED_FACE('',(#803),#676,.F.);
#11243=ADVANCED_FACE('',(#804),#10957,.F.);
#11244=ADVANCED_FACE('',(#805),#677,.F.);
#11245=ADVANCED_FACE('',(#806),#104,.F.);
#11246=ADVANCED_FACE('',(#807),#678,.F.);
#11247=ADVANCED_FACE('',(#808),#105,.T.);
#11248=ADVANCED_FACE('',(#809),#679,.T.);
#11249=ADVANCED_FACE('',(#810),#106,.T.);
#11250=ADVANCED_FACE('',(#811),#107,.T.);
#11251=ADVANCED_FACE('',(#812),#680,.T.);
#11252=ADVANCED_FACE('',(#813),#108,.T.);
#11253=ADVANCED_FACE('',(#814),#223,.T.);
#11254=ADVANCED_FACE('',(#815,#553,#554),#224,.T.);
#11255=ADVANCED_FACE('',(#816),#225,.T.);
#11256=ADVANCED_FACE('',(#817),#226,.F.);
#11257=ADVANCED_FACE('',(#818),#227,.F.);
#11258=ADVANCED_FACE('',(#819),#228,.F.);
#11259=ADVANCED_FACE('',(#820),#229,.T.);
#11260=ADVANCED_FACE('',(#821),#230,.T.);
#11261=ADVANCED_FACE('',(#822),#231,.F.);
#11262=ADVANCED_FACE('',(#823),#232,.T.);
#11263=ADVANCED_FACE('',(#824),#233,.F.);
#11264=ADVANCED_FACE('',(#825),#234,.T.);
#11265=ADVANCED_FACE('',(#826),#235,.F.);
#11266=ADVANCED_FACE('',(#827),#236,.T.);
#11267=ADVANCED_FACE('',(#828),#237,.F.);
#11268=ADVANCED_FACE('',(#829),#238,.T.);
#11269=ADVANCED_FACE('',(#830),#239,.F.);
#11270=ADVANCED_FACE('',(#831),#240,.F.);
#11271=ADVANCED_FACE('',(#832),#241,.T.);
#11272=ADVANCED_FACE('',(#833),#242,.T.);
#11273=ADVANCED_FACE('',(#834),#243,.F.);
#11274=ADVANCED_FACE('',(#835),#244,.F.);
#11275=ADVANCED_FACE('',(#836),#245,.T.);
#11276=ADVANCED_FACE('',(#837,#555,#556,#557,#558,#559,#560,#561),#246,
 .F.);
#11277=ADVANCED_FACE('',(#838,#562,#563,#564,#565,#566,#567,#568),#247,
 .T.);
#11278=ADVANCED_FACE('',(#839),#10958,.F.);
#11279=ADVANCED_FACE('',(#840),#10959,.T.);
#11280=ADVANCED_FACE('',(#841),#681,.F.);
#11281=ADVANCED_FACE('',(#842),#638,.T.);
#11282=ADVANCED_FACE('',(#843),#639,.T.);
#11283=ADVANCED_FACE('',(#844),#682,.F.);
#11284=ADVANCED_FACE('',(#845),#109,.F.);
#11285=ADVANCED_FACE('',(#846),#10960,.F.);
#11286=ADVANCED_FACE('',(#847),#10961,.T.);
#11287=ADVANCED_FACE('',(#848),#10962,.T.);
#11288=ADVANCED_FACE('',(#849),#10963,.T.);
#11289=ADVANCED_FACE('',(#850),#10964,.T.);
#11290=ADVANCED_FACE('',(#851),#10965,.T.);
#11291=ADVANCED_FACE('',(#852),#10966,.T.);
#11292=ADVANCED_FACE('',(#853),#10967,.F.);
#11293=ADVANCED_FACE('',(#854),#10968,.T.);
#11294=ADVANCED_FACE('',(#855),#10969,.F.);
#11295=ADVANCED_FACE('',(#856),#110,.F.);
#11296=ADVANCED_FACE('',(#857),#640,.T.);
#11297=ADVANCED_FACE('',(#858),#641,.T.);
#11298=ADVANCED_FACE('',(#859),#642,.T.);
#11299=ADVANCED_FACE('',(#860),#683,.F.);
#11300=ADVANCED_FACE('',(#861),#111,.F.);
#11301=ADVANCED_FACE('',(#862),#684,.F.);
#11302=ADVANCED_FACE('',(#863),#10970,.T.);
#11303=ADVANCED_FACE('',(#864),#10971,.T.);
#11304=ADVANCED_FACE('',(#865),#10972,.T.);
#11305=ADVANCED_FACE('',(#866),#10973,.T.);
#11306=ADVANCED_FACE('',(#867),#10974,.F.);
#11307=ADVANCED_FACE('',(#868),#685,.F.);
#11308=ADVANCED_FACE('',(#869),#112,.F.);
#11309=ADVANCED_FACE('',(#870),#643,.T.);
#11310=ADVANCED_FACE('',(#871),#644,.T.);
#11311=ADVANCED_FACE('',(#872),#10975,.F.);
#11312=ADVANCED_FACE('',(#873),#10976,.T.);
#11313=ADVANCED_FACE('',(#874),#10977,.T.);
#11314=ADVANCED_FACE('',(#875),#10978,.T.);
#11315=ADVANCED_FACE('',(#876),#10979,.F.);
#11316=ADVANCED_FACE('',(#877),#10980,.F.);
#11317=ADVANCED_FACE('',(#878),#113,.F.);
#11318=ADVANCED_FACE('',(#879),#645,.T.);
#11319=ADVANCED_FACE('',(#880),#686,.F.);
#11320=ADVANCED_FACE('',(#881),#687,.F.);
#11321=ADVANCED_FACE('',(#882),#10981,.T.);
#11322=ADVANCED_FACE('',(#883),#10982,.F.);
#11323=ADVANCED_FACE('',(#884),#10983,.T.);
#11324=ADVANCED_FACE('',(#885),#688,.F.);
#11325=ADVANCED_FACE('',(#886),#114,.F.);
#11326=ADVANCED_FACE('',(#887),#689,.F.);
#11327=ADVANCED_FACE('',(#888),#115,.F.);
#11328=ADVANCED_FACE('',(#889),#10984,.F.);
#11329=ADVANCED_FACE('',(#890),#10985,.F.);
#11330=ADVANCED_FACE('',(#891),#10986,.T.);
#11331=ADVANCED_FACE('',(#892),#10987,.F.);
#11332=ADVANCED_FACE('',(#893),#116,.F.);
#11333=ADVANCED_FACE('',(#894),#690,.F.);
#11334=ADVANCED_FACE('',(#895),#646,.T.);
#11335=ADVANCED_FACE('',(#896),#10988,.T.);
#11336=ADVANCED_FACE('',(#897),#10989,.T.);
#11337=ADVANCED_FACE('',(#898),#10990,.T.);
#11338=ADVANCED_FACE('',(#899),#10991,.T.);
#11339=ADVANCED_FACE('',(#900),#10992,.T.);
#11340=ADVANCED_FACE('',(#901),#647,.T.);
#11341=ADVANCED_FACE('',(#902),#648,.T.);
#11342=ADVANCED_FACE('',(#903),#649,.T.);
#11343=ADVANCED_FACE('',(#904),#650,.T.);
#11344=ADVANCED_FACE('',(#905),#10993,.T.);
#11345=ADVANCED_FACE('',(#906),#10994,.T.);
#11346=ADVANCED_FACE('',(#907),#10995,.T.);
#11347=ADVANCED_FACE('',(#908),#10996,.T.);
#11348=ADVANCED_FACE('',(#909),#10997,.T.);
#11349=ADVANCED_FACE('',(#910),#691,.F.);
#11350=ADVANCED_FACE('',(#911),#117,.F.);
#11351=ADVANCED_FACE('',(#912),#651,.T.);
#11352=ADVANCED_FACE('',(#913),#652,.T.);
#11353=ADVANCED_FACE('',(#914),#118,.F.);
#11354=ADVANCED_FACE('',(#915),#10998,.T.);
#11355=ADVANCED_FACE('',(#916),#10999,.T.);
#11356=ADVANCED_FACE('',(#917),#11000,.T.);
#11357=ADVANCED_FACE('',(#918),#11001,.F.);
#11358=ADVANCED_FACE('',(#919),#653,.F.);
#11359=ADVANCED_FACE('',(#920),#654,.T.);
#11360=ADVANCED_FACE('',(#921),#119,.F.);
#11361=ADVANCED_FACE('',(#922),#692,.F.);
#11362=ADVANCED_FACE('',(#923),#11002,.T.);
#11363=ADVANCED_FACE('',(#924),#11003,.F.);
#11364=ADVANCED_FACE('',(#925),#11004,.T.);
#11365=ADVANCED_FACE('',(#926),#693,.F.);
#11366=ADVANCED_FACE('',(#927),#120,.F.);
#11367=ADVANCED_FACE('',(#928),#694,.F.);
#11368=ADVANCED_FACE('',(#929),#121,.F.);
#11369=ADVANCED_FACE('',(#930),#11005,.F.);
#11370=ADVANCED_FACE('',(#931),#11006,.T.);
#11371=ADVANCED_FACE('',(#932),#11007,.F.);
#11372=ADVANCED_FACE('',(#933),#11008,.F.);
#11373=ADVANCED_FACE('',(#934),#122,.F.);
#11374=ADVANCED_FACE('',(#935),#695,.F.);
#11375=ADVANCED_FACE('',(#936),#696,.F.);
#11376=ADVANCED_FACE('',(#937),#655,.F.);
#11377=ADVANCED_FACE('',(#938),#697,.F.);
#11378=ADVANCED_FACE('',(#939),#11009,.F.);
#11379=ADVANCED_FACE('',(#940),#11010,.F.);
#11380=ADVANCED_FACE('',(#941),#11011,.T.);
#11381=ADVANCED_FACE('',(#942),#698,.F.);
#11382=ADVANCED_FACE('',(#943),#656,.F.);
#11383=ADVANCED_FACE('',(#944),#699,.F.);
#11384=ADVANCED_FACE('',(#945),#123,.F.);
#11385=ADVANCED_FACE('',(#946),#11012,.F.);
#11386=ADVANCED_FACE('',(#947),#11013,.T.);
#11387=ADVANCED_FACE('',(#948),#11014,.F.);
#11388=ADVANCED_FACE('',(#949),#657,.F.);
#11389=ADVANCED_FACE('',(#950),#124,.F.);
#11390=ADVANCED_FACE('',(#951),#700,.F.);
#11391=ADVANCED_FACE('',(#952),#625,.T.);
#11392=ADVANCED_FACE('',(#953),#626,.T.);
#11393=ADVANCED_FACE('',(#954),#627,.T.);
#11394=ADVANCED_FACE('',(#955),#11015,.F.);
#11395=ADVANCED_FACE('',(#956),#11016,.F.);
#11396=ADVANCED_FACE('',(#957,#569,#570,#571,#572,#573,#574,#575,#576,#577),
#11017,.T.);
#11397=ADVANCED_FACE('',(#958),#11018,.T.);
#11398=ADVANCED_FACE('',(#959),#11019,.T.);
#11399=ADVANCED_FACE('',(#960),#248,.T.);
#11400=ADVANCED_FACE('',(#961),#249,.T.);
#11401=ADVANCED_FACE('',(#962),#250,.T.);
#11402=ADVANCED_FACE('',(#963),#251,.T.);
#11403=ADVANCED_FACE('',(#964),#252,.T.);
#11404=ADVANCED_FACE('',(#965),#253,.T.);
#11405=ADVANCED_FACE('',(#966),#254,.T.);
#11406=ADVANCED_FACE('',(#967),#255,.T.);
#11407=ADVANCED_FACE('',(#968),#256,.T.);
#11408=ADVANCED_FACE('',(#969),#257,.T.);
#11409=ADVANCED_FACE('',(#970,#578),#258,.T.);
#11410=ADVANCED_FACE('',(#971,#579),#259,.F.);
#11411=ADVANCED_FACE('',(#972,#580),#260,.F.);
#11412=ADVANCED_FACE('',(#973,#581),#261,.F.);
#11413=ADVANCED_FACE('',(#974),#262,.F.);
#11414=ADVANCED_FACE('',(#975),#263,.F.);
#11415=ADVANCED_FACE('',(#976),#11020,.F.);
#11416=ADVANCED_FACE('',(#977),#264,.F.);
#11417=ADVANCED_FACE('',(#978),#265,.F.);
#11418=ADVANCED_FACE('',(#979),#11021,.T.);
#11419=ADVANCED_FACE('',(#980),#266,.F.);
#11420=ADVANCED_FACE('',(#981),#267,.F.);
#11421=ADVANCED_FACE('',(#982),#11022,.F.);
#11422=ADVANCED_FACE('',(#983),#268,.F.);
#11423=ADVANCED_FACE('',(#984),#269,.F.);
#11424=ADVANCED_FACE('',(#985),#270,.F.);
#11425=ADVANCED_FACE('',(#986),#271,.F.);
#11426=ADVANCED_FACE('',(#987),#11023,.F.);
#11427=ADVANCED_FACE('',(#988),#272,.F.);
#11428=ADVANCED_FACE('',(#989),#273,.F.);
#11429=ADVANCED_FACE('',(#990),#274,.F.);
#11430=ADVANCED_FACE('',(#991),#275,.F.);
#11431=ADVANCED_FACE('',(#992),#11024,.F.);
#11432=ADVANCED_FACE('',(#993),#276,.F.);
#11433=ADVANCED_FACE('',(#994),#277,.F.);
#11434=ADVANCED_FACE('',(#995),#278,.F.);
#11435=ADVANCED_FACE('',(#996),#279,.F.);
#11436=ADVANCED_FACE('',(#997),#11025,.F.);
#11437=ADVANCED_FACE('',(#998),#280,.F.);
#11438=ADVANCED_FACE('',(#999),#281,.F.);
#11439=ADVANCED_FACE('',(#1000),#282,.F.);
#11440=ADVANCED_FACE('',(#1001),#283,.F.);
#11441=ADVANCED_FACE('',(#1002),#11026,.F.);
#11442=ADVANCED_FACE('',(#1003),#284,.F.);
#11443=ADVANCED_FACE('',(#1004),#285,.F.);
#11444=ADVANCED_FACE('',(#1005),#286,.F.);
#11445=ADVANCED_FACE('',(#1006),#287,.F.);
#11446=ADVANCED_FACE('',(#1007),#11027,.F.);
#11447=ADVANCED_FACE('',(#1008),#288,.F.);
#11448=ADVANCED_FACE('',(#1009),#289,.F.);
#11449=ADVANCED_FACE('',(#1010),#290,.F.);
#11450=ADVANCED_FACE('',(#1011),#291,.F.);
#11451=ADVANCED_FACE('',(#1012),#11028,.F.);
#11452=ADVANCED_FACE('',(#1013),#292,.F.);
#11453=ADVANCED_FACE('',(#1014),#293,.F.);
#11454=ADVANCED_FACE('',(#1015),#294,.F.);
#11455=ADVANCED_FACE('',(#1016),#295,.F.);
#11456=ADVANCED_FACE('',(#1017),#11029,.F.);
#11457=ADVANCED_FACE('',(#1018),#296,.F.);
#11458=ADVANCED_FACE('',(#1019),#297,.F.);
#11459=ADVANCED_FACE('',(#1020),#298,.F.);
#11460=ADVANCED_FACE('',(#1021),#299,.F.);
#11461=ADVANCED_FACE('',(#1022),#11030,.F.);
#11462=ADVANCED_FACE('',(#1023),#300,.F.);
#11463=ADVANCED_FACE('',(#1024),#301,.F.);
#11464=ADVANCED_FACE('',(#1025),#11031,.T.);
#11465=ADVANCED_FACE('',(#1026),#11032,.T.);
#11466=ADVANCED_FACE('',(#1027),#11033,.T.);
#11467=ADVANCED_FACE('',(#1028),#11034,.T.);
#11468=ADVANCED_FACE('',(#1029),#11035,.T.);
#11469=ADVANCED_FACE('',(#1030),#11036,.T.);
#11470=ADVANCED_FACE('',(#1031),#11037,.T.);
#11471=ADVANCED_FACE('',(#1032),#11038,.T.);
#11472=ADVANCED_FACE('',(#1033),#11039,.T.);
#11473=ADVANCED_FACE('',(#1034),#302,.F.);
#11474=ADVANCED_FACE('',(#1035),#303,.F.);
#11475=ADVANCED_FACE('',(#1036),#304,.F.);
#11476=ADVANCED_FACE('',(#1037),#305,.F.);
#11477=ADVANCED_FACE('',(#1038),#306,.F.);
#11478=ADVANCED_FACE('',(#1039),#307,.F.);
#11479=ADVANCED_FACE('',(#1040),#308,.F.);
#11480=ADVANCED_FACE('',(#1041),#309,.F.);
#11481=ADVANCED_FACE('',(#1042),#310,.F.);
#11482=ADVANCED_FACE('',(#1043),#311,.F.);
#11483=ADVANCED_FACE('',(#1044,#582),#312,.T.);
#11484=ADVANCED_FACE('',(#1045),#313,.F.);
#11485=ADVANCED_FACE('',(#1046),#314,.F.);
#11486=ADVANCED_FACE('',(#1047),#315,.F.);
#11487=ADVANCED_FACE('',(#1048),#701,.T.);
#11488=ADVANCED_FACE('',(#1049),#702,.T.);
#11489=ADVANCED_FACE('',(#1050),#628,.F.);
#11490=ADVANCED_FACE('',(#1051),#11040,.F.);
#11491=ADVANCED_FACE('',(#1052),#629,.F.);
#11492=ADVANCED_FACE('',(#1053),#11041,.F.);
#11493=ADVANCED_FACE('',(#1054),#630,.F.);
#11494=ADVANCED_FACE('',(#1055),#11042,.F.);
#11495=ADVANCED_FACE('',(#1056),#631,.F.);
#11496=ADVANCED_FACE('',(#1057),#11043,.F.);
#11497=ADVANCED_FACE('',(#1058),#632,.F.);
#11498=ADVANCED_FACE('',(#1059),#11044,.F.);
#11499=ADVANCED_FACE('',(#1060),#633,.F.);
#11500=ADVANCED_FACE('',(#1061),#11045,.F.);
#11501=ADVANCED_FACE('',(#1062),#11046,.F.);
#11502=ADVANCED_FACE('',(#1063),#11047,.T.);
#11503=ADVANCED_FACE('',(#1064,#583,#584,#585,#586,#587,#588,#589),#316,
 .T.);
#11504=ADVANCED_FACE('',(#1065,#590,#591,#592,#593,#594,#595,#596),#317,
 .F.);
#11505=ADVANCED_FACE('',(#1066),#318,.F.);
#11506=ADVANCED_FACE('',(#1067),#319,.F.);
#11507=ADVANCED_FACE('',(#1068),#11048,.T.);
#11508=ADVANCED_FACE('',(#1069),#320,.F.);
#11509=ADVANCED_FACE('',(#1070),#11049,.F.);
#11510=ADVANCED_FACE('',(#1071),#321,.F.);
#11511=ADVANCED_FACE('',(#1072),#11050,.F.);
#11512=ADVANCED_FACE('',(#1073),#322,.F.);
#11513=ADVANCED_FACE('',(#1074),#11051,.T.);
#11514=ADVANCED_FACE('',(#1075),#323,.F.);
#11515=ADVANCED_FACE('',(#1076),#324,.F.);
#11516=ADVANCED_FACE('',(#1077),#325,.F.);
#11517=ADVANCED_FACE('',(#1078),#326,.T.);
#11518=ADVANCED_FACE('',(#1079),#327,.T.);
#11519=ADVANCED_FACE('',(#1080),#328,.T.);
#11520=ADVANCED_FACE('',(#1081),#329,.F.);
#11521=ADVANCED_FACE('',(#1082),#330,.F.);
#11522=ADVANCED_FACE('',(#1083),#331,.F.);
#11523=ADVANCED_FACE('',(#1084),#11052,.T.);
#11524=ADVANCED_FACE('',(#1085),#332,.F.);
#11525=ADVANCED_FACE('',(#1086),#11053,.F.);
#11526=ADVANCED_FACE('',(#1087),#333,.F.);
#11527=ADVANCED_FACE('',(#1088),#11054,.F.);
#11528=ADVANCED_FACE('',(#1089),#334,.F.);
#11529=ADVANCED_FACE('',(#1090),#11055,.T.);
#11530=ADVANCED_FACE('',(#1091),#335,.F.);
#11531=ADVANCED_FACE('',(#1092),#336,.F.);
#11532=ADVANCED_FACE('',(#1093),#337,.F.);
#11533=ADVANCED_FACE('',(#1094),#338,.T.);
#11534=ADVANCED_FACE('',(#1095),#339,.F.);
#11535=ADVANCED_FACE('',(#1096),#340,.F.);
#11536=ADVANCED_FACE('',(#1097),#341,.F.);
#11537=ADVANCED_FACE('',(#1098),#11056,.T.);
#11538=ADVANCED_FACE('',(#1099),#342,.F.);
#11539=ADVANCED_FACE('',(#1100),#11057,.F.);
#11540=ADVANCED_FACE('',(#1101),#343,.F.);
#11541=ADVANCED_FACE('',(#1102),#11058,.F.);
#11542=ADVANCED_FACE('',(#1103),#344,.F.);
#11543=ADVANCED_FACE('',(#1104),#11059,.T.);
#11544=ADVANCED_FACE('',(#1105),#345,.F.);
#11545=ADVANCED_FACE('',(#1106),#346,.F.);
#11546=ADVANCED_FACE('',(#1107),#347,.F.);
#11547=ADVANCED_FACE('',(#1108),#348,.F.);
#11548=ADVANCED_FACE('',(#1109),#349,.F.);
#11549=ADVANCED_FACE('',(#1110),#11060,.T.);
#11550=ADVANCED_FACE('',(#1111),#350,.F.);
#11551=ADVANCED_FACE('',(#1112),#11061,.F.);
#11552=ADVANCED_FACE('',(#1113),#351,.F.);
#11553=ADVANCED_FACE('',(#1114),#11062,.F.);
#11554=ADVANCED_FACE('',(#1115),#352,.F.);
#11555=ADVANCED_FACE('',(#1116),#11063,.T.);
#11556=ADVANCED_FACE('',(#1117),#353,.F.);
#11557=ADVANCED_FACE('',(#1118),#354,.F.);
#11558=ADVANCED_FACE('',(#1119),#355,.F.);
#11559=ADVANCED_FACE('',(#1120),#356,.T.);
#11560=ADVANCED_FACE('',(#1121),#357,.T.);
#11561=ADVANCED_FACE('',(#1122),#358,.F.);
#11562=ADVANCED_FACE('',(#1123),#359,.F.);
#11563=ADVANCED_FACE('',(#1124),#11064,.T.);
#11564=ADVANCED_FACE('',(#1125),#360,.F.);
#11565=ADVANCED_FACE('',(#1126),#11065,.F.);
#11566=ADVANCED_FACE('',(#1127),#361,.F.);
#11567=ADVANCED_FACE('',(#1128),#11066,.F.);
#11568=ADVANCED_FACE('',(#1129),#362,.F.);
#11569=ADVANCED_FACE('',(#1130),#11067,.T.);
#11570=ADVANCED_FACE('',(#1131),#363,.F.);
#11571=ADVANCED_FACE('',(#1132),#364,.F.);
#11572=ADVANCED_FACE('',(#1133),#365,.F.);
#11573=ADVANCED_FACE('',(#1134),#366,.T.);
#11574=ADVANCED_FACE('',(#1135),#367,.T.);
#11575=ADVANCED_FACE('',(#1136),#368,.T.);
#11576=ADVANCED_FACE('',(#1137),#369,.F.);
#11577=ADVANCED_FACE('',(#1138),#370,.F.);
#11578=ADVANCED_FACE('',(#1139),#371,.F.);
#11579=ADVANCED_FACE('',(#1140),#11068,.T.);
#11580=ADVANCED_FACE('',(#1141),#372,.F.);
#11581=ADVANCED_FACE('',(#1142),#11069,.F.);
#11582=ADVANCED_FACE('',(#1143),#373,.F.);
#11583=ADVANCED_FACE('',(#1144),#11070,.F.);
#11584=ADVANCED_FACE('',(#1145),#374,.F.);
#11585=ADVANCED_FACE('',(#1146),#11071,.T.);
#11586=ADVANCED_FACE('',(#1147),#375,.F.);
#11587=ADVANCED_FACE('',(#1148),#376,.F.);
#11588=ADVANCED_FACE('',(#1149),#377,.F.);
#11589=ADVANCED_FACE('',(#1150),#378,.F.);
#11590=ADVANCED_FACE('',(#1151),#379,.F.);
#11591=ADVANCED_FACE('',(#1152),#11072,.T.);
#11592=ADVANCED_FACE('',(#1153),#380,.F.);
#11593=ADVANCED_FACE('',(#1154),#11073,.F.);
#11594=ADVANCED_FACE('',(#1155),#381,.F.);
#11595=ADVANCED_FACE('',(#1156),#11074,.F.);
#11596=ADVANCED_FACE('',(#1157),#382,.F.);
#11597=ADVANCED_FACE('',(#1158),#11075,.T.);
#11598=ADVANCED_FACE('',(#1159),#383,.F.);
#11599=ADVANCED_FACE('',(#1160),#384,.F.);
#11600=ADVANCED_FACE('',(#1161),#385,.F.);
#11601=ADVANCED_FACE('',(#1162),#386,.T.);
#11602=ADVANCED_FACE('',(#1163),#387,.T.);
#11603=ADVANCED_FACE('',(#1164),#388,.T.);
#11604=ADVANCED_FACE('',(#1165),#389,.F.);
#11605=ADVANCED_FACE('',(#1166),#390,.F.);
#11606=ADVANCED_FACE('',(#1167),#391,.F.);
#11607=ADVANCED_FACE('',(#1168),#11076,.T.);
#11608=ADVANCED_FACE('',(#1169),#392,.F.);
#11609=ADVANCED_FACE('',(#1170),#11077,.F.);
#11610=ADVANCED_FACE('',(#1171),#393,.F.);
#11611=ADVANCED_FACE('',(#1172),#11078,.F.);
#11612=ADVANCED_FACE('',(#1173),#394,.F.);
#11613=ADVANCED_FACE('',(#1174),#11079,.T.);
#11614=ADVANCED_FACE('',(#1175),#395,.F.);
#11615=ADVANCED_FACE('',(#1176),#396,.F.);
#11616=ADVANCED_FACE('',(#1177),#397,.F.);
#11617=ADVANCED_FACE('',(#1178),#398,.T.);
#11618=ADVANCED_FACE('',(#1179),#399,.F.);
#11619=ADVANCED_FACE('',(#1180),#400,.F.);
#11620=ADVANCED_FACE('',(#1181),#401,.F.);
#11621=ADVANCED_FACE('',(#1182),#11080,.T.);
#11622=ADVANCED_FACE('',(#1183),#402,.F.);
#11623=ADVANCED_FACE('',(#1184),#11081,.F.);
#11624=ADVANCED_FACE('',(#1185),#403,.F.);
#11625=ADVANCED_FACE('',(#1186),#11082,.F.);
#11626=ADVANCED_FACE('',(#1187),#404,.F.);
#11627=ADVANCED_FACE('',(#1188),#11083,.T.);
#11628=ADVANCED_FACE('',(#1189),#405,.F.);
#11629=ADVANCED_FACE('',(#1190),#406,.F.);
#11630=ADVANCED_FACE('',(#1191),#407,.F.);
#11631=ADVANCED_FACE('',(#1192),#408,.F.);
#11632=ADVANCED_FACE('',(#1193),#409,.F.);
#11633=ADVANCED_FACE('',(#1194),#410,.F.);
#11634=ADVANCED_FACE('',(#1195),#411,.F.);
#11635=ADVANCED_FACE('',(#1196),#11084,.T.);
#11636=ADVANCED_FACE('',(#1197),#412,.F.);
#11637=ADVANCED_FACE('',(#1198),#11085,.F.);
#11638=ADVANCED_FACE('',(#1199),#413,.F.);
#11639=ADVANCED_FACE('',(#1200),#11086,.F.);
#11640=ADVANCED_FACE('',(#1201),#414,.F.);
#11641=ADVANCED_FACE('',(#1202),#11087,.T.);
#11642=ADVANCED_FACE('',(#1203),#415,.F.);
#11643=ADVANCED_FACE('',(#1204),#416,.F.);
#11644=ADVANCED_FACE('',(#1205),#417,.F.);
#11645=ADVANCED_FACE('',(#1206),#418,.F.);
#11646=ADVANCED_FACE('',(#1207),#419,.F.);
#11647=ADVANCED_FACE('',(#1208),#11088,.T.);
#11648=ADVANCED_FACE('',(#1209),#420,.F.);
#11649=ADVANCED_FACE('',(#1210),#11089,.F.);
#11650=ADVANCED_FACE('',(#1211),#421,.F.);
#11651=ADVANCED_FACE('',(#1212),#11090,.T.);
#11652=ADVANCED_FACE('',(#1213),#422,.F.);
#11653=ADVANCED_FACE('',(#1214),#423,.F.);
#11654=ADVANCED_FACE('',(#1215),#424,.F.);
#11655=ADVANCED_FACE('',(#1216),#425,.T.);
#11656=ADVANCED_FACE('',(#1217),#426,.F.);
#11657=ADVANCED_FACE('',(#1218),#427,.F.);
#11658=ADVANCED_FACE('',(#1219),#11091,.T.);
#11659=ADVANCED_FACE('',(#1220),#428,.F.);
#11660=ADVANCED_FACE('',(#1221),#11092,.F.);
#11661=ADVANCED_FACE('',(#1222),#429,.F.);
#11662=ADVANCED_FACE('',(#1223),#11093,.T.);
#11663=ADVANCED_FACE('',(#1224),#430,.F.);
#11664=ADVANCED_FACE('',(#1225),#431,.F.);
#11665=ADVANCED_FACE('',(#1226),#432,.F.);
#11666=ADVANCED_FACE('',(#1227),#433,.T.);
#11667=ADVANCED_FACE('',(#1228),#434,.F.);
#11668=ADVANCED_FACE('',(#1229),#435,.F.);
#11669=ADVANCED_FACE('',(#1230),#11094,.T.);
#11670=ADVANCED_FACE('',(#1231),#436,.F.);
#11671=ADVANCED_FACE('',(#1232),#11095,.F.);
#11672=ADVANCED_FACE('',(#1233),#437,.F.);
#11673=ADVANCED_FACE('',(#1234),#11096,.T.);
#11674=ADVANCED_FACE('',(#1235),#438,.F.);
#11675=ADVANCED_FACE('',(#1236),#439,.F.);
#11676=ADVANCED_FACE('',(#1237),#440,.F.);
#11677=ADVANCED_FACE('',(#1238),#441,.T.);
#11678=ADVANCED_FACE('',(#1239),#442,.F.);
#11679=ADVANCED_FACE('',(#1240),#443,.F.);
#11680=ADVANCED_FACE('',(#1241),#11097,.T.);
#11681=ADVANCED_FACE('',(#1242),#444,.F.);
#11682=ADVANCED_FACE('',(#1243),#11098,.F.);
#11683=ADVANCED_FACE('',(#1244),#445,.F.);
#11684=ADVANCED_FACE('',(#1245),#11099,.T.);
#11685=ADVANCED_FACE('',(#1246),#446,.F.);
#11686=ADVANCED_FACE('',(#1247),#447,.F.);
#11687=ADVANCED_FACE('',(#1248),#448,.F.);
#11688=ADVANCED_FACE('',(#1249),#449,.T.);
#11689=ADVANCED_FACE('',(#1250),#450,.F.);
#11690=ADVANCED_FACE('',(#1251),#451,.F.);
#11691=ADVANCED_FACE('',(#1252),#452,.F.);
#11692=ADVANCED_FACE('',(#1253),#11100,.T.);
#11693=ADVANCED_FACE('',(#1254),#453,.F.);
#11694=ADVANCED_FACE('',(#1255),#11101,.F.);
#11695=ADVANCED_FACE('',(#1256),#454,.F.);
#11696=ADVANCED_FACE('',(#1257),#11102,.T.);
#11697=ADVANCED_FACE('',(#1258),#455,.F.);
#11698=ADVANCED_FACE('',(#1259),#456,.F.);
#11699=ADVANCED_FACE('',(#1260),#457,.F.);
#11700=ADVANCED_FACE('',(#1261),#458,.F.);
#11701=ADVANCED_FACE('',(#1262),#459,.F.);
#11702=ADVANCED_FACE('',(#1263),#11103,.T.);
#11703=ADVANCED_FACE('',(#1264),#460,.F.);
#11704=ADVANCED_FACE('',(#1265),#11104,.F.);
#11705=ADVANCED_FACE('',(#1266),#461,.F.);
#11706=ADVANCED_FACE('',(#1267),#11105,.T.);
#11707=ADVANCED_FACE('',(#1268),#462,.F.);
#11708=ADVANCED_FACE('',(#1269),#463,.F.);
#11709=ADVANCED_FACE('',(#1270),#464,.T.);
#11710=ADVANCED_FACE('',(#1271),#465,.T.);
#11711=ADVANCED_FACE('',(#1272),#466,.T.);
#11712=ADVANCED_FACE('',(#1273),#467,.F.);
#11713=ADVANCED_FACE('',(#1274),#468,.F.);
#11714=ADVANCED_FACE('',(#1275),#11106,.T.);
#11715=ADVANCED_FACE('',(#1276),#469,.F.);
#11716=ADVANCED_FACE('',(#1277),#11107,.F.);
#11717=ADVANCED_FACE('',(#1278),#470,.F.);
#11718=ADVANCED_FACE('',(#1279),#11108,.T.);
#11719=ADVANCED_FACE('',(#1280),#471,.F.);
#11720=ADVANCED_FACE('',(#1281),#472,.F.);
#11721=ADVANCED_FACE('',(#1282),#473,.F.);
#11722=ADVANCED_FACE('',(#1283),#474,.T.);
#11723=ADVANCED_FACE('',(#1284),#475,.F.);
#11724=ADVANCED_FACE('',(#1285),#476,.F.);
#11725=ADVANCED_FACE('',(#1286),#11109,.T.);
#11726=ADVANCED_FACE('',(#1287),#477,.F.);
#11727=ADVANCED_FACE('',(#1288),#11110,.F.);
#11728=ADVANCED_FACE('',(#1289),#478,.F.);
#11729=ADVANCED_FACE('',(#1290),#11111,.T.);
#11730=ADVANCED_FACE('',(#1291),#479,.F.);
#11731=ADVANCED_FACE('',(#1292),#480,.F.);
#11732=ADVANCED_FACE('',(#1293),#481,.F.);
#11733=ADVANCED_FACE('',(#1294),#482,.F.);
#11734=ADVANCED_FACE('',(#1295),#483,.F.);
#11735=ADVANCED_FACE('',(#1296),#11112,.T.);
#11736=ADVANCED_FACE('',(#1297),#484,.F.);
#11737=ADVANCED_FACE('',(#1298),#11113,.F.);
#11738=ADVANCED_FACE('',(#1299),#485,.F.);
#11739=ADVANCED_FACE('',(#1300),#11114,.T.);
#11740=ADVANCED_FACE('',(#1301),#486,.F.);
#11741=ADVANCED_FACE('',(#1302),#487,.F.);
#11742=ADVANCED_FACE('',(#1303),#488,.T.);
#11743=ADVANCED_FACE('',(#1304),#489,.T.);
#11744=ADVANCED_FACE('',(#1305),#490,.F.);
#11745=ADVANCED_FACE('',(#1306),#491,.F.);
#11746=ADVANCED_FACE('',(#1307),#492,.F.);
#11747=ADVANCED_FACE('',(#1308),#11115,.T.);
#11748=ADVANCED_FACE('',(#1309),#493,.F.);
#11749=ADVANCED_FACE('',(#1310),#11116,.F.);
#11750=ADVANCED_FACE('',(#1311),#494,.F.);
#11751=ADVANCED_FACE('',(#1312),#11117,.T.);
#11752=ADVANCED_FACE('',(#1313),#495,.F.);
#11753=ADVANCED_FACE('',(#1314),#496,.F.);
#11754=ADVANCED_FACE('',(#1315),#497,.F.);
#11755=ADVANCED_FACE('',(#1316),#11118,.F.);
#11756=ADVANCED_FACE('',(#1317),#11119,.F.);
#11757=ADVANCED_FACE('',(#1318),#11120,.F.);
#11758=ADVANCED_FACE('',(#1319),#11121,.F.);
#11759=ADVANCED_FACE('',(#1320),#498,.F.);
#11760=ADVANCED_FACE('',(#1321),#499,.F.);
#11761=ADVANCED_FACE('',(#1322),#500,.F.);
#11762=ADVANCED_FACE('',(#1323),#501,.F.);
#11763=ADVANCED_FACE('',(#1324,#597,#598,#599,#600),#502,.F.);
#11764=ADVANCED_FACE('',(#1325,#601,#602,#603,#604),#503,.T.);
#11765=ADVANCED_FACE('',(#1326),#504,.F.);
#11766=ADVANCED_FACE('',(#1327),#11122,.F.);
#11767=ADVANCED_FACE('',(#1328),#505,.F.);
#11768=ADVANCED_FACE('',(#1329),#506,.F.);
#11769=ADVANCED_FACE('',(#1330),#11123,.F.);
#11770=ADVANCED_FACE('',(#1331),#507,.F.);
#11771=ADVANCED_FACE('',(#1332),#508,.F.);
#11772=ADVANCED_FACE('',(#1333),#11124,.F.);
#11773=ADVANCED_FACE('',(#1334),#509,.F.);
#11774=ADVANCED_FACE('',(#1335),#510,.F.);
#11775=ADVANCED_FACE('',(#1336),#11125,.F.);
#11776=ADVANCED_FACE('',(#1337),#511,.F.);
#11777=ADVANCED_FACE('',(#1338),#512,.F.);
#11778=ADVANCED_FACE('',(#1339),#513,.F.);
#11779=ADVANCED_FACE('',(#1340),#514,.F.);
#11780=ADVANCED_FACE('',(#1341),#515,.F.);
#11781=ADVANCED_FACE('',(#1342),#11126,.F.);
#11782=ADVANCED_FACE('',(#1343),#11127,.F.);
#11783=ADVANCED_FACE('',(#1344),#516,.F.);
#11784=ADVANCED_FACE('',(#1345),#517,.F.);
#11785=ADVANCED_FACE('',(#1346),#11128,.T.);
#11786=ADVANCED_FACE('',(#1347),#518,.F.);
#11787=ADVANCED_FACE('',(#1348),#11129,.F.);
#11788=ADVANCED_FACE('',(#1349,#605,#606),#519,.F.);
#11789=ADVANCED_FACE('',(#1350),#11130,.F.);
#11790=ADVANCED_FACE('',(#1351),#520,.F.);
#11791=ADVANCED_FACE('',(#1352),#11131,.T.);
#11792=ADVANCED_FACE('',(#1353),#521,.F.);
#11793=ADVANCED_FACE('',(#1354),#522,.F.);
#11794=ADVANCED_FACE('',(#1355,#607,#608),#523,.F.);
#11795=ADVANCED_FACE('',(#1356),#524,.T.);
#11796=ADVANCED_FACE('',(#1357),#525,.T.);
#11797=ADVANCED_FACE('',(#1358),#11132,.F.);
#11798=ADVANCED_FACE('',(#1359),#11133,.F.);
#11799=ADVANCED_FACE('',(#1360,#609,#610),#526,.F.);
#11800=ADVANCED_FACE('',(#1361),#527,.F.);
#11801=ADVANCED_FACE('',(#1362),#11134,.T.);
#11802=ADVANCED_FACE('',(#1363,#611,#612),#528,.F.);
#11803=ADVANCED_FACE('',(#1364),#11135,.F.);
#11804=ADVANCED_FACE('',(#1365),#529,.F.);
#11805=ADVANCED_FACE('',(#1366),#11136,.T.);
#11806=ADVANCED_FACE('',(#1367),#530,.F.);
#11807=ADVANCED_FACE('',(#1368),#531,.F.);
#11808=ADVANCED_FACE('',(#1369),#532,.F.);
#11809=ADVANCED_FACE('',(#1370),#533,.T.);
#11810=ADVANCED_FACE('',(#1371),#11137,.F.);
#11811=ADVANCED_FACE('',(#1372),#11138,.F.);
#11812=ADVANCED_FACE('',(#1373,#613,#614),#534,.F.);
#11813=ADVANCED_FACE('',(#1374),#535,.F.);
#11814=ADVANCED_FACE('',(#1375),#11139,.T.);
#11815=ADVANCED_FACE('',(#1376,#615,#616),#536,.F.);
#11816=ADVANCED_FACE('',(#1377),#11140,.F.);
#11817=ADVANCED_FACE('',(#1378),#537,.F.);
#11818=ADVANCED_FACE('',(#1379),#11141,.T.);
#11819=ADVANCED_FACE('',(#1380),#538,.F.);
#11820=ADVANCED_FACE('',(#1381),#539,.F.);
#11821=ADVANCED_FACE('',(#1382),#540,.F.);
#11822=ADVANCED_FACE('',(#1383),#541,.T.);
#11823=CLOSED_SHELL('',(#11142,#11143,#11144,#11145,#11146,#11147,#11148,
#11149,#11150,#11151,#11152,#11153,#11154,#11155,#11156,#11157,#11158,#11159,
#11160,#11161,#11162,#11163,#11164,#11165,#11166,#11167,#11168,#11169,#11170,
#11171,#11172,#11173,#11174,#11175,#11176,#11177,#11178,#11179,#11180,#11181,
#11182,#11183,#11184,#11185,#11186,#11187,#11188,#11189,#11190,#11191,#11192,
#11193,#11194,#11195,#11196,#11197,#11198,#11199,#11200,#11201,#11202,#11203,
#11204,#11205,#11206,#11207,#11208,#11209,#11210,#11211,#11212,#11213,#11214,
#11215,#11216,#11217,#11218,#11219,#11220,#11221,#11222,#11223,#11224,#11225,
#11226,#11227,#11228,#11229,#11230,#11231,#11232,#11233,#11234,#11235,#11236,
#11237,#11238,#11239,#11240,#11241,#11242,#11243,#11244,#11245,#11246,#11247,
#11248,#11249,#11250,#11251,#11252,#11253,#11254,#11255,#11256,#11257,#11258,
#11259,#11260,#11261,#11262,#11263,#11264,#11265,#11266,#11267,#11268,#11269,
#11270,#11271,#11272,#11273,#11274,#11275,#11276,#11277,#11278,#11279,#11280,
#11281,#11282,#11283,#11284,#11285,#11286,#11287,#11288,#11289,#11290,#11291,
#11292,#11293,#11294,#11295,#11296,#11297,#11298,#11299,#11300,#11301,#11302,
#11303,#11304,#11305,#11306,#11307,#11308,#11309,#11310,#11311,#11312,#11313,
#11314,#11315,#11316,#11317,#11318,#11319,#11320,#11321,#11322,#11323,#11324,
#11325,#11326,#11327,#11328,#11329,#11330,#11331,#11332,#11333,#11334,#11335,
#11336,#11337,#11338,#11339,#11340,#11341,#11342,#11343,#11344,#11345,#11346,
#11347,#11348,#11349,#11350,#11351,#11352,#11353,#11354,#11355,#11356,#11357,
#11358,#11359,#11360,#11361,#11362,#11363,#11364,#11365,#11366,#11367,#11368,
#11369,#11370,#11371,#11372,#11373,#11374,#11375,#11376,#11377,#11378,#11379,
#11380,#11381,#11382,#11383,#11384,#11385,#11386,#11387,#11388,#11389,#11390));
#11824=CLOSED_SHELL('',(#11391,#11392,#11393,#11394,#11395,#11396,#11397,
#11398,#11399,#11400,#11401,#11402,#11403,#11404,#11405,#11406,#11407,#11408,
#11409,#11410,#11411,#11412,#11413,#11414,#11415,#11416,#11417,#11418,#11419,
#11420,#11421,#11422,#11423,#11424,#11425,#11426,#11427,#11428,#11429,#11430,
#11431,#11432,#11433,#11434,#11435,#11436,#11437,#11438,#11439,#11440,#11441,
#11442,#11443,#11444,#11445,#11446,#11447,#11448,#11449,#11450,#11451,#11452,
#11453,#11454,#11455,#11456,#11457,#11458,#11459,#11460,#11461,#11462,#11463,
#11464,#11465,#11466,#11467,#11468,#11469,#11470,#11471,#11472,#11473,#11474,
#11475,#11476,#11477,#11478,#11479,#11480,#11481,#11482,#11483,#11484,#11485,
#11486));
#11825=CLOSED_SHELL('',(#11487,#11488,#11489,#11490,#11491,#11492,#11493,
#11494,#11495,#11496,#11497,#11498,#11499,#11500,#11501,#11502,#11503,#11504));
#11826=CLOSED_SHELL('',(#11505,#11506,#11507,#11508,#11509,#11510,#11511,
#11512,#11513,#11514,#11515,#11516,#11517,#11518));
#11827=CLOSED_SHELL('',(#11519,#11520,#11521,#11522,#11523,#11524,#11525,
#11526,#11527,#11528,#11529,#11530,#11531,#11532));
#11828=CLOSED_SHELL('',(#11533,#11534,#11535,#11536,#11537,#11538,#11539,
#11540,#11541,#11542,#11543,#11544,#11545,#11546));
#11829=CLOSED_SHELL('',(#11547,#11548,#11549,#11550,#11551,#11552,#11553,
#11554,#11555,#11556,#11557,#11558,#11559,#11560));
#11830=CLOSED_SHELL('',(#11561,#11562,#11563,#11564,#11565,#11566,#11567,
#11568,#11569,#11570,#11571,#11572,#11573,#11574));
#11831=CLOSED_SHELL('',(#11575,#11576,#11577,#11578,#11579,#11580,#11581,
#11582,#11583,#11584,#11585,#11586,#11587,#11588));
#11832=CLOSED_SHELL('',(#11589,#11590,#11591,#11592,#11593,#11594,#11595,
#11596,#11597,#11598,#11599,#11600,#11601,#11602));
#11833=CLOSED_SHELL('',(#11603,#11604,#11605,#11606,#11607,#11608,#11609,
#11610,#11611,#11612,#11613,#11614,#11615,#11616));
#11834=CLOSED_SHELL('',(#11617,#11618,#11619,#11620,#11621,#11622,#11623,
#11624,#11625,#11626,#11627,#11628,#11629,#11630));
#11835=CLOSED_SHELL('',(#11631,#11632,#11633,#11634,#11635,#11636,#11637,
#11638,#11639,#11640,#11641,#11642,#11643,#11644));
#11836=CLOSED_SHELL('',(#11645,#11646,#11647,#11648,#11649,#11650,#11651,
#11652,#11653,#11654,#11655));
#11837=CLOSED_SHELL('',(#11656,#11657,#11658,#11659,#11660,#11661,#11662,
#11663,#11664,#11665,#11666));
#11838=CLOSED_SHELL('',(#11667,#11668,#11669,#11670,#11671,#11672,#11673,
#11674,#11675,#11676,#11677));
#11839=CLOSED_SHELL('',(#11678,#11679,#11680,#11681,#11682,#11683,#11684,
#11685,#11686,#11687,#11688));
#11840=CLOSED_SHELL('',(#11689,#11690,#11691,#11692,#11693,#11694,#11695,
#11696,#11697,#11698,#11699));
#11841=CLOSED_SHELL('',(#11700,#11701,#11702,#11703,#11704,#11705,#11706,
#11707,#11708,#11709,#11710));
#11842=CLOSED_SHELL('',(#11711,#11712,#11713,#11714,#11715,#11716,#11717,
#11718,#11719,#11720,#11721));
#11843=CLOSED_SHELL('',(#11722,#11723,#11724,#11725,#11726,#11727,#11728,
#11729,#11730,#11731,#11732));
#11844=CLOSED_SHELL('',(#11733,#11734,#11735,#11736,#11737,#11738,#11739,
#11740,#11741,#11742,#11743));
#11845=CLOSED_SHELL('',(#11744,#11745,#11746,#11747,#11748,#11749,#11750,
#11751,#11752,#11753,#11754));
#11846=CLOSED_SHELL('',(#11755,#11756,#11757,#11758,#11759,#11760,#11761,
#11762,#11763,#11764,#11765,#11766,#11767,#11768,#11769,#11770,#11771,#11772,
#11773,#11774,#11775,#11776,#11777,#11778,#11779,#11780));
#11847=CLOSED_SHELL('',(#11781,#11782,#11783,#11784,#11785,#11786,#11787,
#11788,#11789,#11790,#11791,#11792,#11793,#11794,#11795,#11796));
#11848=CLOSED_SHELL('',(#11797,#11798,#11799,#11800,#11801,#11802,#11803,
#11804,#11805,#11806,#11807,#11808,#11809));
#11849=CLOSED_SHELL('',(#11810,#11811,#11812,#11813,#11814,#11815,#11816,
#11817,#11818,#11819,#11820,#11821,#11822));
#11850=DERIVED_UNIT_ELEMENT(#11858,1.);
#11851=DERIVED_UNIT_ELEMENT(#27543,-3.);
#11852=DERIVED_UNIT_ELEMENT(#11858,1.);
#11853=DERIVED_UNIT_ELEMENT(#27543,-3.);
#11854=DERIVED_UNIT_ELEMENT(#11858,1.);
#11855=DERIVED_UNIT_ELEMENT(#27543,-3.);
#11856=DERIVED_UNIT_ELEMENT(#11858,1.);
#11857=DERIVED_UNIT_ELEMENT(#27543,-3.);
#11858=(
MASS_UNIT()
NAMED_UNIT(*)
SI_UNIT(.KILO.,.GRAM.)
);
#11859=DERIVED_UNIT((#11850,#11851));
#11860=DERIVED_UNIT((#11852,#11853));
#11861=DERIVED_UNIT((#11854,#11855));
#11862=DERIVED_UNIT((#11856,#11857));
#11863=MEASURE_REPRESENTATION_ITEM('density measure',
POSITIVE_RATIO_MEASURE(7850.),#11859);
#11864=MEASURE_REPRESENTATION_ITEM('density measure',
POSITIVE_RATIO_MEASURE(7850.),#11860);
#11865=MEASURE_REPRESENTATION_ITEM('density measure',
POSITIVE_RATIO_MEASURE(7850.),#11861);
#11866=MEASURE_REPRESENTATION_ITEM('density measure',
POSITIVE_RATIO_MEASURE(7850.),#11862);
#11867=PROPERTY_DEFINITION_REPRESENTATION(#11887,#11875);
#11868=PROPERTY_DEFINITION_REPRESENTATION(#11888,#11876);
#11869=PROPERTY_DEFINITION_REPRESENTATION(#11889,#11877);
#11870=PROPERTY_DEFINITION_REPRESENTATION(#11890,#11878);
#11871=PROPERTY_DEFINITION_REPRESENTATION(#11891,#11879);
#11872=PROPERTY_DEFINITION_REPRESENTATION(#11892,#11880);
#11873=PROPERTY_DEFINITION_REPRESENTATION(#11893,#11881);
#11874=PROPERTY_DEFINITION_REPRESENTATION(#11894,#11882);
#11875=REPRESENTATION('material name',(#11883),#27537);
#11876=REPRESENTATION('density',(#11863),#27537);
#11877=REPRESENTATION('material name',(#11884),#27538);
#11878=REPRESENTATION('density',(#11864),#27538);
#11879=REPRESENTATION('material name',(#11885),#27539);
#11880=REPRESENTATION('density',(#11865),#27539);
#11881=REPRESENTATION('material name',(#11886),#27540);
#11882=REPRESENTATION('density',(#11866),#27540);
#11883=DESCRIPTIVE_REPRESENTATION_ITEM('Steel','Steel');
#11884=DESCRIPTIVE_REPRESENTATION_ITEM('Steel','Steel');
#11885=DESCRIPTIVE_REPRESENTATION_ITEM('Steel','Steel');
#11886=DESCRIPTIVE_REPRESENTATION_ITEM('Steel','Steel');
#11887=PROPERTY_DEFINITION('material property','material name',#27567);
#11888=PROPERTY_DEFINITION('material property','density of part',#27567);
#11889=PROPERTY_DEFINITION('material property','material name',#27568);
#11890=PROPERTY_DEFINITION('material property','density of part',#27568);
#11891=PROPERTY_DEFINITION('material property','material name',#27569);
#11892=PROPERTY_DEFINITION('material property','density of part',#27569);
#11893=PROPERTY_DEFINITION('material property','material name',#27570);
#11894=PROPERTY_DEFINITION('material property','density of part',#27570);
#11895=AXIS2_PLACEMENT_3D('',#16753,#13177,#13178);
#11896=AXIS2_PLACEMENT_3D('',#16754,#13179,#13180);
#11897=AXIS2_PLACEMENT_3D('',#16755,#13181,#13182);
#11898=AXIS2_PLACEMENT_3D('',#16806,#13184,#13185);
#11899=AXIS2_PLACEMENT_3D('',#16807,#13186,#13187);
#11900=AXIS2_PLACEMENT_3D('',#16810,#13188,#13189);
#11901=AXIS2_PLACEMENT_3D('',#16811,#13190,#13191);
#11902=AXIS2_PLACEMENT_3D('',#16813,#13192,#13193);
#11903=AXIS2_PLACEMENT_3D('',#16814,#13194,#13195);
#11904=AXIS2_PLACEMENT_3D('',#16815,#13196,#13197);
#11905=AXIS2_PLACEMENT_3D('',#16818,#13198,#13199);
#11906=AXIS2_PLACEMENT_3D('',#16822,#13201,#13202);
#11907=AXIS2_PLACEMENT_3D('',#16824,#13204,#13205);
#11908=AXIS2_PLACEMENT_3D('',#16827,#13206,#13207);
#11909=AXIS2_PLACEMENT_3D('',#16829,#13208,#13209);
#11910=AXIS2_PLACEMENT_3D('',#16833,#13211,#13212);
#11911=AXIS2_PLACEMENT_3D('',#16835,#13214,#13215);
#11912=AXIS2_PLACEMENT_3D('',#16838,#13216,#13217);
#11913=AXIS2_PLACEMENT_3D('',#16842,#13219,#13220);
#11914=AXIS2_PLACEMENT_3D('',#16844,#13222,#13223);
#11915=AXIS2_PLACEMENT_3D('',#16847,#13224,#13225);
#11916=AXIS2_PLACEMENT_3D('',#16849,#13226,#13227);
#11917=AXIS2_PLACEMENT_3D('',#16850,#13228,#13229);
#11918=AXIS2_PLACEMENT_3D('',#16851,#13230,#13231);
#11919=AXIS2_PLACEMENT_3D('',#16854,#13232,#13233);
#11920=AXIS2_PLACEMENT_3D('',#16856,#13234,#13235);
#11921=AXIS2_PLACEMENT_3D('',#16857,#13236,#13237);
#11922=AXIS2_PLACEMENT_3D('',#16858,#13238,#13239);
#11923=AXIS2_PLACEMENT_3D('',#16861,#13240,#13241);
#11924=AXIS2_PLACEMENT_3D('',#16863,#13242,#13243);
#11925=AXIS2_PLACEMENT_3D('',#16864,#13244,#13245);
#11926=AXIS2_PLACEMENT_3D('',#16865,#13246,#13247);
#11927=AXIS2_PLACEMENT_3D('',#16868,#13248,#13249);
#11928=AXIS2_PLACEMENT_3D('',#16870,#13250,#13251);
#11929=AXIS2_PLACEMENT_3D('',#16871,#13252,#13253);
#11930=AXIS2_PLACEMENT_3D('',#16872,#13254,#13255);
#11931=AXIS2_PLACEMENT_3D('',#16874,#13256,#13257);
#11932=AXIS2_PLACEMENT_3D('',#16876,#13258,#13259);
#11933=AXIS2_PLACEMENT_3D('',#16878,#13260,#13261);
#11934=AXIS2_PLACEMENT_3D('',#16879,#13262,#13263);
#11935=AXIS2_PLACEMENT_3D('',#16880,#13264,#13265);
#11936=AXIS2_PLACEMENT_3D('',#16883,#13266,#13267);
#11937=AXIS2_PLACEMENT_3D('',#16884,#13268,#13269);
#11938=AXIS2_PLACEMENT_3D('',#16886,#13270,#13271);
#11939=AXIS2_PLACEMENT_3D('',#16887,#13272,#13273);
#11940=AXIS2_PLACEMENT_3D('',#16888,#13274,#13275);
#11941=AXIS2_PLACEMENT_3D('',#16890,#13276,#13277);
#11942=AXIS2_PLACEMENT_3D('',#16893,#13279,#13280);
#11943=AXIS2_PLACEMENT_3D('',#16894,#13281,#13282);
#11944=AXIS2_PLACEMENT_3D('',#16896,#13283,#13284);
#11945=AXIS2_PLACEMENT_3D('',#16898,#13286,#13287);
#11946=AXIS2_PLACEMENT_3D('',#16900,#13288,#13289);
#11947=AXIS2_PLACEMENT_3D('',#16903,#13291,#13292);
#11948=AXIS2_PLACEMENT_3D('',#16904,#13293,#13294);
#11949=AXIS2_PLACEMENT_3D('',#16906,#13295,#13296);
#11950=AXIS2_PLACEMENT_3D('',#16908,#13298,#13299);
#11951=AXIS2_PLACEMENT_3D('',#16910,#13300,#13301);
#11952=AXIS2_PLACEMENT_3D('',#16913,#13303,#13304);
#11953=AXIS2_PLACEMENT_3D('',#16914,#13305,#13306);
#11954=AXIS2_PLACEMENT_3D('',#16916,#13307,#13308);
#11955=AXIS2_PLACEMENT_3D('',#16918,#13310,#13311);
#11956=AXIS2_PLACEMENT_3D('',#16920,#13312,#13313);
#11957=AXIS2_PLACEMENT_3D('',#16923,#13315,#13316);
#11958=AXIS2_PLACEMENT_3D('',#16924,#13317,#13318);
#11959=AXIS2_PLACEMENT_3D('',#16926,#13319,#13320);
#11960=AXIS2_PLACEMENT_3D('',#16928,#13322,#13323);
#11961=AXIS2_PLACEMENT_3D('',#16930,#13324,#13325);
#11962=AXIS2_PLACEMENT_3D('',#16933,#13327,#13328);
#11963=AXIS2_PLACEMENT_3D('',#16934,#13329,#13330);
#11964=AXIS2_PLACEMENT_3D('',#16936,#13331,#13332);
#11965=AXIS2_PLACEMENT_3D('',#16938,#13334,#13335);
#11966=AXIS2_PLACEMENT_3D('',#16940,#13336,#13337);
#11967=AXIS2_PLACEMENT_3D('',#16943,#13339,#13340);
#11968=AXIS2_PLACEMENT_3D('',#16944,#13341,#13342);
#11969=AXIS2_PLACEMENT_3D('',#16946,#13343,#13344);
#11970=AXIS2_PLACEMENT_3D('',#16948,#13346,#13347);
#11971=AXIS2_PLACEMENT_3D('',#16950,#13349,#13350);
#11972=AXIS2_PLACEMENT_3D('',#16952,#13351,#13352);
#11973=AXIS2_PLACEMENT_3D('',#16955,#13354,#13355);
#11974=AXIS2_PLACEMENT_3D('',#16956,#13356,#13357);
#11975=AXIS2_PLACEMENT_3D('',#16959,#13358,#13359);
#11976=AXIS2_PLACEMENT_3D('',#16960,#13360,#13361);
#11977=AXIS2_PLACEMENT_3D('',#16963,#13363,#13364);
#11978=AXIS2_PLACEMENT_3D('',#16964,#13365,#13366);
#11979=AXIS2_PLACEMENT_3D('',#16966,#13368,#13369);
#11980=AXIS2_PLACEMENT_3D('',#16968,#13370,#13371);
#11981=AXIS2_PLACEMENT_3D('',#16971,#13373,#13374);
#11982=AXIS2_PLACEMENT_3D('',#16972,#13375,#13376);
#11983=AXIS2_PLACEMENT_3D('',#16974,#13377,#13378);
#11984=AXIS2_PLACEMENT_3D('',#16977,#13380,#13381);
#11985=AXIS2_PLACEMENT_3D('',#16978,#13382,#13383);
#11986=AXIS2_PLACEMENT_3D('',#16980,#13384,#13385);
#11987=AXIS2_PLACEMENT_3D('',#16983,#13387,#13388);
#11988=AXIS2_PLACEMENT_3D('',#16984,#13389,#13390);
#11989=AXIS2_PLACEMENT_3D('',#16986,#13391,#13392);
#11990=AXIS2_PLACEMENT_3D('',#16989,#13394,#13395);
#11991=AXIS2_PLACEMENT_3D('',#16990,#13396,#13397);
#11992=AXIS2_PLACEMENT_3D('',#16993,#13398,#13399);
#11993=AXIS2_PLACEMENT_3D('',#16997,#13401,#13402);
#11994=AXIS2_PLACEMENT_3D('',#16999,#13404,#13405);
#11995=AXIS2_PLACEMENT_3D('',#17001,#13406,#13407);
#11996=AXIS2_PLACEMENT_3D('',#17303,#13408,#13409);
#11997=AXIS2_PLACEMENT_3D('',#17353,#13411,#13412);
#11998=AXIS2_PLACEMENT_3D('',#17355,#13414,#13415);
#11999=AXIS2_PLACEMENT_3D('',#17358,#13416,#13417);
#12000=AXIS2_PLACEMENT_3D('',#17360,#13418,#13419);
#12001=AXIS2_PLACEMENT_3D('',#17364,#13421,#13422);
#12002=AXIS2_PLACEMENT_3D('',#17366,#13423,#13424);
#12003=AXIS2_PLACEMENT_3D('',#17368,#13426,#13427);
#12004=AXIS2_PLACEMENT_3D('',#17375,#13431,#13432);
#12005=AXIS2_PLACEMENT_3D('',#17424,#13433,#13434);
#12006=AXIS2_PLACEMENT_3D('',#17741,#13435,#13436);
#12007=AXIS2_PLACEMENT_3D('',#17789,#13437,#13438);
#12008=AXIS2_PLACEMENT_3D('',#17958,#13440,#13441);
#12009=AXIS2_PLACEMENT_3D('',#18046,#13442,#13443);
#12010=AXIS2_PLACEMENT_3D('',#18207,#13445,#13446);
#12011=AXIS2_PLACEMENT_3D('',#18291,#13447,#13448);
#12012=AXIS2_PLACEMENT_3D('',#18460,#13450,#13451);
#12013=AXIS2_PLACEMENT_3D('',#18462,#13452,#13453);
#12014=AXIS2_PLACEMENT_3D('',#18631,#13455,#13456);
#12015=AXIS2_PLACEMENT_3D('',#18634,#13458,#13459);
#12016=AXIS2_PLACEMENT_3D('',#18803,#13461,#13462);
#12017=AXIS2_PLACEMENT_3D('',#18893,#13464,#13465);
#12018=AXIS2_PLACEMENT_3D('',#19054,#13467,#13468);
#12019=AXIS2_PLACEMENT_3D('',#19139,#13470,#13471);
#12020=AXIS2_PLACEMENT_3D('',#19152,#13478,#13479);
#12021=AXIS2_PLACEMENT_3D('',#19166,#13486,#13487);
#12022=AXIS2_PLACEMENT_3D('',#19170,#13489,#13490);
#12023=AXIS2_PLACEMENT_3D('',#19176,#13494,#13495);
#12024=AXIS2_PLACEMENT_3D('',#19180,#13497,#13498);
#12025=AXIS2_PLACEMENT_3D('',#19185,#13502,#13503);
#12026=AXIS2_PLACEMENT_3D('',#19200,#13511,#13512);
#12027=AXIS2_PLACEMENT_3D('',#19204,#13514,#13515);
#12028=AXIS2_PLACEMENT_3D('',#19209,#13518,#13519);
#12029=AXIS2_PLACEMENT_3D('',#19212,#13521,#13522);
#12030=AXIS2_PLACEMENT_3D('',#19213,#13523,#13524);
#12031=AXIS2_PLACEMENT_3D('',#19214,#13525,#13526);
#12032=AXIS2_PLACEMENT_3D('',#19216,#13527,#13528);
#12033=AXIS2_PLACEMENT_3D('',#19218,#13529,#13530);
#12034=AXIS2_PLACEMENT_3D('',#19220,#13532,#13533);
#12035=AXIS2_PLACEMENT_3D('',#19223,#13534,#13535);
#12036=AXIS2_PLACEMENT_3D('',#19225,#13536,#13537);
#12037=AXIS2_PLACEMENT_3D('',#19227,#13538,#13539);
#12038=AXIS2_PLACEMENT_3D('',#19230,#13541,#13542);
#12039=AXIS2_PLACEMENT_3D('',#19231,#13543,#13544);
#12040=AXIS2_PLACEMENT_3D('',#19233,#13545,#13546);
#12041=AXIS2_PLACEMENT_3D('',#19235,#13547,#13548);
#12042=AXIS2_PLACEMENT_3D('',#19239,#13550,#13551);
#12043=AXIS2_PLACEMENT_3D('',#19240,#13552,#13553);
#12044=AXIS2_PLACEMENT_3D('',#19241,#13554,#13555);
#12045=AXIS2_PLACEMENT_3D('',#19244,#13556,#13557);
#12046=AXIS2_PLACEMENT_3D('',#19246,#13558,#13559);
#12047=AXIS2_PLACEMENT_3D('',#19248,#13560,#13561);
#12048=AXIS2_PLACEMENT_3D('',#19250,#13562,#13563);
#12049=AXIS2_PLACEMENT_3D('',#19252,#13565,#13566);
#12050=AXIS2_PLACEMENT_3D('',#19257,#13568,#13569);
#12051=AXIS2_PLACEMENT_3D('',#19261,#13571,#13572);
#12052=AXIS2_PLACEMENT_3D('',#19265,#13574,#13575);
#12053=AXIS2_PLACEMENT_3D('',#19268,#13577,#13578);
#12054=AXIS2_PLACEMENT_3D('',#19273,#13580,#13581);
#12055=AXIS2_PLACEMENT_3D('',#19277,#13583,#13584);
#12056=AXIS2_PLACEMENT_3D('',#19281,#13586,#13587);
#12057=AXIS2_PLACEMENT_3D('',#19284,#13589,#13590);
#12058=AXIS2_PLACEMENT_3D('',#19285,#13591,#13592);
#12059=AXIS2_PLACEMENT_3D('',#19287,#13593,#13594);
#12060=AXIS2_PLACEMENT_3D('',#19291,#13597,#13598);
#12061=AXIS2_PLACEMENT_3D('',#19292,#13599,#13600);
#12062=AXIS2_PLACEMENT_3D('',#19296,#13602,#13603);
#12063=AXIS2_PLACEMENT_3D('',#19300,#13606,#13607);
#12064=AXIS2_PLACEMENT_3D('',#19305,#13609,#13610);
#12065=AXIS2_PLACEMENT_3D('',#19308,#13613,#13614);
#12066=AXIS2_PLACEMENT_3D('',#19314,#13618,#13619);
#12067=AXIS2_PLACEMENT_3D('',#19329,#13620,#13621);
#12068=AXIS2_PLACEMENT_3D('',#19330,#13622,#13623);
#12069=AXIS2_PLACEMENT_3D('',#19331,#13624,#13625);
#12070=AXIS2_PLACEMENT_3D('',#19347,#13626,#13627);
#12071=AXIS2_PLACEMENT_3D('',#19349,#13628,#13629);
#12072=AXIS2_PLACEMENT_3D('',#19364,#13630,#13631);
#12073=AXIS2_PLACEMENT_3D('',#19365,#13632,#13633);
#12074=AXIS2_PLACEMENT_3D('',#19366,#13634,#13635);
#12075=AXIS2_PLACEMENT_3D('',#19381,#13636,#13637);
#12076=AXIS2_PLACEMENT_3D('',#19382,#13638,#13639);
#12077=AXIS2_PLACEMENT_3D('',#19383,#13640,#13641);
#12078=AXIS2_PLACEMENT_3D('',#19384,#13642,#13643);
#12079=AXIS2_PLACEMENT_3D('',#19397,#13644,#13645);
#12080=AXIS2_PLACEMENT_3D('',#19416,#13646,#13647);
#12081=AXIS2_PLACEMENT_3D('',#19417,#13648,#13649);
#12082=AXIS2_PLACEMENT_3D('',#19418,#13650,#13651);
#12083=AXIS2_PLACEMENT_3D('',#19419,#13652,#13653);
#12084=AXIS2_PLACEMENT_3D('',#19607,#13654,#13655);
#12085=AXIS2_PLACEMENT_3D('',#19608,#13656,#13657);
#12086=AXIS2_PLACEMENT_3D('',#19621,#13658,#13659);
#12087=AXIS2_PLACEMENT_3D('',#19640,#13660,#13661);
#12088=AXIS2_PLACEMENT_3D('',#19641,#13662,#13663);
#12089=AXIS2_PLACEMENT_3D('',#19642,#13664,#13665);
#12090=AXIS2_PLACEMENT_3D('',#19643,#13666,#13667);
#12091=AXIS2_PLACEMENT_3D('',#19831,#13668,#13669);
#12092=AXIS2_PLACEMENT_3D('',#19832,#13670,#13671);
#12093=AXIS2_PLACEMENT_3D('',#19833,#13672,#13673);
#12094=AXIS2_PLACEMENT_3D('',#19834,#13674,#13675);
#12095=AXIS2_PLACEMENT_3D('',#19847,#13676,#13677);
#12096=AXIS2_PLACEMENT_3D('',#19848,#13678,#13679);
#12097=AXIS2_PLACEMENT_3D('',#20009,#13680,#13681);
#12098=AXIS2_PLACEMENT_3D('',#20010,#13682,#13683);
#12099=AXIS2_PLACEMENT_3D('',#20011,#13684,#13685);
#12100=AXIS2_PLACEMENT_3D('',#20012,#13686,#13687);
#12101=AXIS2_PLACEMENT_3D('',#20025,#13688,#13689);
#12102=AXIS2_PLACEMENT_3D('',#20026,#13690,#13691);
#12103=AXIS2_PLACEMENT_3D('',#20322,#13692,#13693);
#12104=AXIS2_PLACEMENT_3D('',#20323,#13694,#13695);
#12105=AXIS2_PLACEMENT_3D('',#20324,#13696,#13697);
#12106=AXIS2_PLACEMENT_3D('',#20595,#13698,#13699);
#12107=AXIS2_PLACEMENT_3D('',#20596,#13700,#13701);
#12108=AXIS2_PLACEMENT_3D('',#20597,#13702,#13703);
#12109=AXIS2_PLACEMENT_3D('',#20724,#13704,#13705);
#12110=AXIS2_PLACEMENT_3D('',#20725,#13706,#13707);
#12111=AXIS2_PLACEMENT_3D('',#20726,#13708,#13709);
#12112=AXIS2_PLACEMENT_3D('',#20728,#13710,#13711);
#12113=AXIS2_PLACEMENT_3D('',#20731,#13713,#13714);
#12114=AXIS2_PLACEMENT_3D('',#20732,#13715,#13716);
#12115=AXIS2_PLACEMENT_3D('',#20735,#13717,#13718);
#12116=AXIS2_PLACEMENT_3D('',#20737,#13719,#13720);
#12117=AXIS2_PLACEMENT_3D('',#20741,#13722,#13723);
#12118=AXIS2_PLACEMENT_3D('',#20742,#13724,#13725);
#12119=AXIS2_PLACEMENT_3D('',#20743,#13726,#13727);
#12120=AXIS2_PLACEMENT_3D('',#20745,#13728,#13729);
#12121=AXIS2_PLACEMENT_3D('',#20747,#13730,#13731);
#12122=AXIS2_PLACEMENT_3D('',#20751,#13733,#13734);
#12123=AXIS2_PLACEMENT_3D('',#20752,#13735,#13736);
#12124=AXIS2_PLACEMENT_3D('',#20753,#13737,#13738);
#12125=AXIS2_PLACEMENT_3D('',#20756,#13739,#13740);
#12126=AXIS2_PLACEMENT_3D('',#20760,#13742,#13743);
#12127=AXIS2_PLACEMENT_3D('',#20762,#13744,#13745);
#12128=AXIS2_PLACEMENT_3D('',#20763,#13746,#13747);
#12129=AXIS2_PLACEMENT_3D('',#20764,#13748,#13749);
#12130=AXIS2_PLACEMENT_3D('',#20766,#13750,#13751);
#12131=AXIS2_PLACEMENT_3D('',#20770,#13754,#13755);
#12132=AXIS2_PLACEMENT_3D('',#20771,#13756,#13757);
#12133=AXIS2_PLACEMENT_3D('',#20778,#13761,#13762);
#12134=AXIS2_PLACEMENT_3D('',#20779,#13763,#13764);
#12135=AXIS2_PLACEMENT_3D('',#20786,#13768,#13769);
#12136=AXIS2_PLACEMENT_3D('',#20787,#13770,#13771);
#12137=AXIS2_PLACEMENT_3D('',#20793,#13775,#13776);
#12138=AXIS2_PLACEMENT_3D('',#20795,#13777,#13778);
#12139=AXIS2_PLACEMENT_3D('',#20796,#13779,#13780);
#12140=AXIS2_PLACEMENT_3D('',#20807,#13781,#13782);
#12141=AXIS2_PLACEMENT_3D('',#20820,#13783,#13784);
#12142=AXIS2_PLACEMENT_3D('',#20822,#13785,#13786);
#12143=AXIS2_PLACEMENT_3D('',#20834,#13787,#13788);
#12144=AXIS2_PLACEMENT_3D('',#20835,#13789,#13790);
#12145=AXIS2_PLACEMENT_3D('',#20836,#13791,#13792);
#12146=AXIS2_PLACEMENT_3D('',#20838,#13793,#13794);
#12147=AXIS2_PLACEMENT_3D('',#20839,#13795,#13796);
#12148=AXIS2_PLACEMENT_3D('',#20850,#13797,#13798);
#12149=AXIS2_PLACEMENT_3D('',#20851,#13799,#13800);
#12150=AXIS2_PLACEMENT_3D('',#20864,#13801,#13802);
#12151=AXIS2_PLACEMENT_3D('',#20883,#13803,#13804);
#12152=AXIS2_PLACEMENT_3D('',#20884,#13805,#13806);
#12153=AXIS2_PLACEMENT_3D('',#20885,#13807,#13808);
#12154=AXIS2_PLACEMENT_3D('',#20886,#13809,#13810);
#12155=AXIS2_PLACEMENT_3D('',#21101,#13811,#13812);
#12156=AXIS2_PLACEMENT_3D('',#21102,#13813,#13814);
#12157=AXIS2_PLACEMENT_3D('',#21115,#13815,#13816);
#12158=AXIS2_PLACEMENT_3D('',#21134,#13817,#13818);
#12159=AXIS2_PLACEMENT_3D('',#21135,#13819,#13820);
#12160=AXIS2_PLACEMENT_3D('',#21136,#13821,#13822);
#12161=AXIS2_PLACEMENT_3D('',#21137,#13823,#13824);
#12162=AXIS2_PLACEMENT_3D('',#21358,#13825,#13826);
#12163=AXIS2_PLACEMENT_3D('',#21359,#13827,#13828);
#12164=AXIS2_PLACEMENT_3D('',#21360,#13829,#13830);
#12165=AXIS2_PLACEMENT_3D('',#21361,#13831,#13832);
#12166=AXIS2_PLACEMENT_3D('',#21374,#13833,#13834);
#12167=AXIS2_PLACEMENT_3D('',#21375,#13835,#13836);
#12168=AXIS2_PLACEMENT_3D('',#21536,#13837,#13838);
#12169=AXIS2_PLACEMENT_3D('',#21537,#13839,#13840);
#12170=AXIS2_PLACEMENT_3D('',#21538,#13841,#13842);
#12171=AXIS2_PLACEMENT_3D('',#21539,#13843,#13844);
#12172=AXIS2_PLACEMENT_3D('',#21552,#13845,#13846);
#12173=AXIS2_PLACEMENT_3D('',#21553,#13847,#13848);
#12174=AXIS2_PLACEMENT_3D('',#21837,#13849,#13850);
#12175=AXIS2_PLACEMENT_3D('',#21838,#13851,#13852);
#12176=AXIS2_PLACEMENT_3D('',#21839,#13853,#13854);
#12177=AXIS2_PLACEMENT_3D('',#22122,#13855,#13856);
#12178=AXIS2_PLACEMENT_3D('',#22123,#13857,#13858);
#12179=AXIS2_PLACEMENT_3D('',#22124,#13859,#13860);
#12180=AXIS2_PLACEMENT_3D('',#22251,#13861,#13862);
#12181=AXIS2_PLACEMENT_3D('',#22260,#13867,#13868);
#12182=AXIS2_PLACEMENT_3D('',#22273,#13875,#13876);
#12183=AXIS2_PLACEMENT_3D('',#22281,#13880,#13881);
#12184=AXIS2_PLACEMENT_3D('',#22282,#13882,#13883);
#12185=AXIS2_PLACEMENT_3D('',#22287,#13885,#13886);
#12186=AXIS2_PLACEMENT_3D('',#22291,#13889,#13890);
#12187=AXIS2_PLACEMENT_3D('',#22300,#13895,#13896);
#12188=AXIS2_PLACEMENT_3D('',#22305,#13898,#13899);
#12189=AXIS2_PLACEMENT_3D('',#22307,#13901,#13902);
#12190=AXIS2_PLACEMENT_3D('',#22312,#13904,#13905);
#12191=AXIS2_PLACEMENT_3D('',#22314,#13907,#13908);
#12192=AXIS2_PLACEMENT_3D('',#22323,#13913,#13914);
#12193=AXIS2_PLACEMENT_3D('',#22328,#13916,#13917);
#12194=AXIS2_PLACEMENT_3D('',#22330,#13919,#13920);
#12195=AXIS2_PLACEMENT_3D('',#22335,#13922,#13923);
#12196=AXIS2_PLACEMENT_3D('',#22337,#13925,#13926);
#12197=AXIS2_PLACEMENT_3D('',#22346,#13931,#13932);
#12198=AXIS2_PLACEMENT_3D('',#22353,#13935,#13936);
#12199=AXIS2_PLACEMENT_3D('',#22355,#13938,#13939);
#12200=AXIS2_PLACEMENT_3D('',#22360,#13941,#13942);
#12201=AXIS2_PLACEMENT_3D('',#22364,#13945,#13946);
#12202=AXIS2_PLACEMENT_3D('',#22373,#13951,#13952);
#12203=AXIS2_PLACEMENT_3D('',#22377,#13954,#13955);
#12204=AXIS2_PLACEMENT_3D('',#22379,#13957,#13958);
#12205=AXIS2_PLACEMENT_3D('',#22383,#13960,#13961);
#12206=AXIS2_PLACEMENT_3D('',#22385,#13963,#13964);
#12207=AXIS2_PLACEMENT_3D('',#22394,#13969,#13970);
#12208=AXIS2_PLACEMENT_3D('',#22398,#13972,#13973);
#12209=AXIS2_PLACEMENT_3D('',#22400,#13975,#13976);
#12210=AXIS2_PLACEMENT_3D('',#22404,#13978,#13979);
#12211=AXIS2_PLACEMENT_3D('',#22406,#13981,#13982);
#12212=AXIS2_PLACEMENT_3D('',#22415,#13987,#13988);
#12213=AXIS2_PLACEMENT_3D('',#22424,#13993,#13994);
#12214=AXIS2_PLACEMENT_3D('',#22433,#13999,#14000);
#12215=AXIS2_PLACEMENT_3D('',#22442,#14005,#14006);
#12216=AXIS2_PLACEMENT_3D('',#22443,#14007,#14008);
#12217=AXIS2_PLACEMENT_3D('',#22444,#14009,#14010);
#12218=AXIS2_PLACEMENT_3D('',#22445,#14011,#14012);
#12219=AXIS2_PLACEMENT_3D('',#22446,#14013,#14014);
#12220=AXIS2_PLACEMENT_3D('',#22553,#14015,#14016);
#12221=AXIS2_PLACEMENT_3D('',#22554,#14017,#14018);
#12222=AXIS2_PLACEMENT_3D('',#22555,#14019,#14020);
#12223=AXIS2_PLACEMENT_3D('',#22556,#14021,#14022);
#12224=AXIS2_PLACEMENT_3D('',#22557,#14023,#14024);
#12225=AXIS2_PLACEMENT_3D('',#22558,#14025,#14026);
#12226=AXIS2_PLACEMENT_3D('',#22559,#14027,#14028);
#12227=AXIS2_PLACEMENT_3D('',#22560,#14029,#14030);
#12228=AXIS2_PLACEMENT_3D('',#22561,#14031,#14032);
#12229=AXIS2_PLACEMENT_3D('',#22562,#14033,#14034);
#12230=AXIS2_PLACEMENT_3D('',#22563,#14035,#14036);
#12231=AXIS2_PLACEMENT_3D('',#22564,#14037,#14038);
#12232=AXIS2_PLACEMENT_3D('',#22565,#14039,#14040);
#12233=AXIS2_PLACEMENT_3D('',#22626,#14041,#14042);
#12234=AXIS2_PLACEMENT_3D('',#22627,#14043,#14044);
#12235=AXIS2_PLACEMENT_3D('',#22628,#14045,#14046);
#12236=AXIS2_PLACEMENT_3D('',#22629,#14047,#14048);
#12237=AXIS2_PLACEMENT_3D('',#22733,#14049,#14050);
#12238=AXIS2_PLACEMENT_3D('',#22734,#14051,#14052);
#12239=AXIS2_PLACEMENT_3D('',#22735,#14053,#14054);
#12240=AXIS2_PLACEMENT_3D('',#22736,#14055,#14056);
#12241=AXIS2_PLACEMENT_3D('',#22737,#14057,#14058);
#12242=AXIS2_PLACEMENT_3D('',#22738,#14059,#14060);
#12243=AXIS2_PLACEMENT_3D('',#22739,#14061,#14062);
#12244=AXIS2_PLACEMENT_3D('',#22740,#14063,#14064);
#12245=AXIS2_PLACEMENT_3D('',#22741,#14065,#14066);
#12246=AXIS2_PLACEMENT_3D('',#22742,#14067,#14068);
#12247=AXIS2_PLACEMENT_3D('',#22743,#14069,#14070);
#12248=AXIS2_PLACEMENT_3D('',#22744,#14071,#14072);
#12249=AXIS2_PLACEMENT_3D('',#22745,#14073,#14074);
#12250=AXIS2_PLACEMENT_3D('',#22861,#14075,#14076);
#12251=AXIS2_PLACEMENT_3D('',#22862,#14077,#14078);
#12252=AXIS2_PLACEMENT_3D('',#22863,#14079,#14080);
#12253=AXIS2_PLACEMENT_3D('',#22930,#14081,#14082);
#12254=AXIS2_PLACEMENT_3D('',#22931,#14083,#14084);
#12255=AXIS2_PLACEMENT_3D('',#22932,#14085,#14086);
#12256=AXIS2_PLACEMENT_3D('',#22933,#14087,#14088);
#12257=AXIS2_PLACEMENT_3D('',#22934,#14089,#14090);
#12258=AXIS2_PLACEMENT_3D('',#22935,#14091,#14092);
#12259=AXIS2_PLACEMENT_3D('',#22936,#14093,#14094);
#12260=AXIS2_PLACEMENT_3D('',#22937,#14095,#14096);
#12261=AXIS2_PLACEMENT_3D('',#22938,#14097,#14098);
#12262=AXIS2_PLACEMENT_3D('',#22939,#14099,#14100);
#12263=AXIS2_PLACEMENT_3D('',#23006,#14101,#14102);
#12264=AXIS2_PLACEMENT_3D('',#23007,#14103,#14104);
#12265=AXIS2_PLACEMENT_3D('',#23008,#14105,#14106);
#12266=AXIS2_PLACEMENT_3D('',#23009,#14107,#14108);
#12267=AXIS2_PLACEMENT_3D('',#23028,#14109,#14110);
#12268=AXIS2_PLACEMENT_3D('',#23029,#14111,#14112);
#12269=AXIS2_PLACEMENT_3D('',#23030,#14113,#14114);
#12270=AXIS2_PLACEMENT_3D('',#23031,#14115,#14116);
#12271=AXIS2_PLACEMENT_3D('',#23032,#14117,#14118);
#12272=AXIS2_PLACEMENT_3D('',#23033,#14119,#14120);
#12273=AXIS2_PLACEMENT_3D('',#23034,#14121,#14122);
#12274=AXIS2_PLACEMENT_3D('',#23035,#14123,#14124);
#12275=AXIS2_PLACEMENT_3D('',#23096,#14125,#14126);
#12276=AXIS2_PLACEMENT_3D('',#23097,#14127,#14128);
#12277=AXIS2_PLACEMENT_3D('',#23098,#14129,#14130);
#12278=AXIS2_PLACEMENT_3D('',#23099,#14131,#14132);
#12279=AXIS2_PLACEMENT_3D('',#23100,#14133,#14134);
#12280=AXIS2_PLACEMENT_3D('',#23101,#14135,#14136);
#12281=AXIS2_PLACEMENT_3D('',#23102,#14137,#14138);
#12282=AXIS2_PLACEMENT_3D('',#23103,#14139,#14140);
#12283=AXIS2_PLACEMENT_3D('',#23104,#14141,#14142);
#12284=AXIS2_PLACEMENT_3D('',#23211,#14143,#14144);
#12285=AXIS2_PLACEMENT_3D('',#23212,#14145,#14146);
#12286=AXIS2_PLACEMENT_3D('',#23213,#14147,#14148);
#12287=AXIS2_PLACEMENT_3D('',#23214,#14149,#14150);
#12288=AXIS2_PLACEMENT_3D('',#23215,#14151,#14152);
#12289=AXIS2_PLACEMENT_3D('',#23216,#14153,#14154);
#12290=AXIS2_PLACEMENT_3D('',#23217,#14155,#14156);
#12291=AXIS2_PLACEMENT_3D('',#23278,#14157,#14158);
#12292=AXIS2_PLACEMENT_3D('',#23279,#14159,#14160);
#12293=AXIS2_PLACEMENT_3D('',#23280,#14161,#14162);
#12294=AXIS2_PLACEMENT_3D('',#23281,#14163,#14164);
#12295=AXIS2_PLACEMENT_3D('',#23282,#14165,#14166);
#12296=AXIS2_PLACEMENT_3D('',#23283,#14167,#14168);
#12297=AXIS2_PLACEMENT_3D('',#23284,#14169,#14170);
#12298=AXIS2_PLACEMENT_3D('',#23285,#14171,#14172);
#12299=AXIS2_PLACEMENT_3D('',#23286,#14173,#14174);
#12300=AXIS2_PLACEMENT_3D('',#23384,#14175,#14176);
#12301=AXIS2_PLACEMENT_3D('',#23385,#14177,#14178);
#12302=AXIS2_PLACEMENT_3D('',#23386,#14179,#14180);
#12303=AXIS2_PLACEMENT_3D('',#23493,#14181,#14182);
#12304=AXIS2_PLACEMENT_3D('',#23494,#14183,#14184);
#12305=AXIS2_PLACEMENT_3D('',#23567,#14185,#14186);
#12306=AXIS2_PLACEMENT_3D('',#23568,#14187,#14188);
#12307=AXIS2_PLACEMENT_3D('',#23569,#14189,#14190);
#12308=AXIS2_PLACEMENT_3D('',#23570,#14191,#14192);
#12309=AXIS2_PLACEMENT_3D('',#23631,#14193,#14194);
#12310=AXIS2_PLACEMENT_3D('',#23632,#14195,#14196);
#12311=AXIS2_PLACEMENT_3D('',#23633,#14197,#14198);
#12312=AXIS2_PLACEMENT_3D('',#23634,#14199,#14200);
#12313=AXIS2_PLACEMENT_3D('',#23750,#14201,#14202);
#12314=AXIS2_PLACEMENT_3D('',#23751,#14203,#14204);
#12315=AXIS2_PLACEMENT_3D('',#23818,#14205,#14206);
#12316=AXIS2_PLACEMENT_3D('',#23819,#14207,#14208);
#12317=AXIS2_PLACEMENT_3D('',#23820,#14209,#14210);
#12318=AXIS2_PLACEMENT_3D('',#23821,#14211,#14212);
#12319=AXIS2_PLACEMENT_3D('',#23822,#14213,#14214);
#12320=AXIS2_PLACEMENT_3D('',#23823,#14215,#14216);
#12321=AXIS2_PLACEMENT_3D('',#23824,#14217,#14218);
#12322=AXIS2_PLACEMENT_3D('',#23825,#14219,#14220);
#12323=AXIS2_PLACEMENT_3D('',#23826,#14221,#14222);
#12324=AXIS2_PLACEMENT_3D('',#23827,#14223,#14224);
#12325=AXIS2_PLACEMENT_3D('',#23828,#14225,#14226);
#12326=AXIS2_PLACEMENT_3D('',#23829,#14227,#14228);
#12327=AXIS2_PLACEMENT_3D('',#23830,#14229,#14230);
#12328=AXIS2_PLACEMENT_3D('',#23831,#14231,#14232);
#12329=AXIS2_PLACEMENT_3D('',#23832,#14233,#14234);
#12330=AXIS2_PLACEMENT_3D('',#23833,#14235,#14236);
#12331=AXIS2_PLACEMENT_3D('',#23834,#14237,#14238);
#12332=AXIS2_PLACEMENT_3D('',#23835,#14239,#14240);
#12333=AXIS2_PLACEMENT_3D('',#23836,#14241,#14242);
#12334=AXIS2_PLACEMENT_3D('',#23837,#14243,#14244);
#12335=AXIS2_PLACEMENT_3D('',#23838,#14245,#14246);
#12336=AXIS2_PLACEMENT_3D('',#23839,#14247,#14248);
#12337=AXIS2_PLACEMENT_3D('',#23840,#14249,#14250);
#12338=AXIS2_PLACEMENT_3D('',#23841,#14251,#14252);
#12339=AXIS2_PLACEMENT_3D('',#23842,#14253,#14254);
#12340=AXIS2_PLACEMENT_3D('',#23843,#14255,#14256);
#12341=AXIS2_PLACEMENT_3D('',#23844,#14257,#14258);
#12342=AXIS2_PLACEMENT_3D('',#23845,#14259,#14260);
#12343=AXIS2_PLACEMENT_3D('',#23943,#14261,#14262);
#12344=AXIS2_PLACEMENT_3D('',#23944,#14263,#14264);
#12345=AXIS2_PLACEMENT_3D('',#23945,#14265,#14266);
#12346=AXIS2_PLACEMENT_3D('',#23946,#14267,#14268);
#12347=AXIS2_PLACEMENT_3D('',#23947,#14269,#14270);
#12348=AXIS2_PLACEMENT_3D('',#23948,#14271,#14272);
#12349=AXIS2_PLACEMENT_3D('',#23949,#14273,#14274);
#12350=AXIS2_PLACEMENT_3D('',#24056,#14275,#14276);
#12351=AXIS2_PLACEMENT_3D('',#24057,#14277,#14278);
#12352=AXIS2_PLACEMENT_3D('',#24058,#14279,#14280);
#12353=AXIS2_PLACEMENT_3D('',#24131,#14281,#14282);
#12354=AXIS2_PLACEMENT_3D('',#24132,#14283,#14284);
#12355=AXIS2_PLACEMENT_3D('',#24133,#14285,#14286);
#12356=AXIS2_PLACEMENT_3D('',#24134,#14287,#14288);
#12357=AXIS2_PLACEMENT_3D('',#24135,#14289,#14290);
#12358=AXIS2_PLACEMENT_3D('',#24196,#14291,#14292);
#12359=AXIS2_PLACEMENT_3D('',#24197,#14293,#14294);
#12360=AXIS2_PLACEMENT_3D('',#24198,#14295,#14296);
#12361=AXIS2_PLACEMENT_3D('',#24199,#14297,#14298);
#12362=AXIS2_PLACEMENT_3D('',#24200,#14299,#14300);
#12363=AXIS2_PLACEMENT_3D('',#24201,#14301,#14302);
#12364=AXIS2_PLACEMENT_3D('',#24220,#14303,#14304);
#12365=AXIS2_PLACEMENT_3D('',#24221,#14305,#14306);
#12366=AXIS2_PLACEMENT_3D('',#24222,#14307,#14308);
#12367=AXIS2_PLACEMENT_3D('',#24223,#14309,#14310);
#12368=AXIS2_PLACEMENT_3D('',#24224,#14311,#14312);
#12369=AXIS2_PLACEMENT_3D('',#24225,#14313,#14314);
#12370=AXIS2_PLACEMENT_3D('',#24226,#14315,#14316);
#12371=AXIS2_PLACEMENT_3D('',#24287,#14317,#14318);
#12372=AXIS2_PLACEMENT_3D('',#24288,#14319,#14320);
#12373=AXIS2_PLACEMENT_3D('',#24289,#14321,#14322);
#12374=AXIS2_PLACEMENT_3D('',#24290,#14323,#14324);
#12375=AXIS2_PLACEMENT_3D('',#24291,#14325,#14326);
#12376=AXIS2_PLACEMENT_3D('',#24407,#14327,#14328);
#12377=AXIS2_PLACEMENT_3D('',#24408,#14329,#14330);
#12378=AXIS2_PLACEMENT_3D('',#24409,#14331,#14332);
#12379=AXIS2_PLACEMENT_3D('',#24513,#14333,#14334);
#12380=AXIS2_PLACEMENT_3D('',#24514,#14335,#14336);
#12381=AXIS2_PLACEMENT_3D('',#24581,#14337,#14338);
#12382=AXIS2_PLACEMENT_3D('',#24582,#14339,#14340);
#12383=AXIS2_PLACEMENT_3D('',#24583,#14341,#14342);
#12384=AXIS2_PLACEMENT_3D('',#24650,#14343,#14344);
#12385=AXIS2_PLACEMENT_3D('',#24651,#14345,#14346);
#12386=AXIS2_PLACEMENT_3D('',#24652,#14347,#14348);
#12387=AXIS2_PLACEMENT_3D('',#24653,#14349,#14350);
#12388=AXIS2_PLACEMENT_3D('',#24760,#14351,#14352);
#12389=AXIS2_PLACEMENT_3D('',#24761,#14353,#14354);
#12390=AXIS2_PLACEMENT_3D('',#24762,#14355,#14356);
#12391=AXIS2_PLACEMENT_3D('',#24763,#14357,#14358);
#12392=AXIS2_PLACEMENT_3D('',#24764,#14359,#14360);
#12393=AXIS2_PLACEMENT_3D('',#24825,#14361,#14362);
#12394=AXIS2_PLACEMENT_3D('',#24826,#14363,#14364);
#12395=AXIS2_PLACEMENT_3D('',#24827,#14365,#14366);
#12396=AXIS2_PLACEMENT_3D('',#24828,#14367,#14368);
#12397=AXIS2_PLACEMENT_3D('',#24829,#14369,#14370);
#12398=AXIS2_PLACEMENT_3D('',#24830,#14371,#14372);
#12399=AXIS2_PLACEMENT_3D('',#24831,#14373,#14374);
#12400=AXIS2_PLACEMENT_3D('',#24832,#14375,#14376);
#12401=AXIS2_PLACEMENT_3D('',#24833,#14377,#14378);
#12402=AXIS2_PLACEMENT_3D('',#24834,#14379,#14380);
#12403=AXIS2_PLACEMENT_3D('',#24835,#14381,#14382);
#12404=AXIS2_PLACEMENT_3D('',#24836,#14383,#14384);
#12405=AXIS2_PLACEMENT_3D('',#24837,#14385,#14386);
#12406=AXIS2_PLACEMENT_3D('',#24838,#14387,#14388);
#12407=AXIS2_PLACEMENT_3D('',#24839,#14389,#14390);
#12408=AXIS2_PLACEMENT_3D('',#24946,#14391,#14392);
#12409=AXIS2_PLACEMENT_3D('',#24947,#14393,#14394);
#12410=AXIS2_PLACEMENT_3D('',#24948,#14395,#14396);
#12411=AXIS2_PLACEMENT_3D('',#24949,#14397,#14398);
#12412=AXIS2_PLACEMENT_3D('',#24950,#14399,#14400);
#12413=AXIS2_PLACEMENT_3D('',#24951,#14401,#14402);
#12414=AXIS2_PLACEMENT_3D('',#25012,#14403,#14404);
#12415=AXIS2_PLACEMENT_3D('',#25013,#14405,#14406);
#12416=AXIS2_PLACEMENT_3D('',#25014,#14407,#14408);
#12417=AXIS2_PLACEMENT_3D('',#25015,#14409,#14410);
#12418=AXIS2_PLACEMENT_3D('',#25131,#14411,#14412);
#12419=AXIS2_PLACEMENT_3D('',#25132,#14413,#14414);
#12420=AXIS2_PLACEMENT_3D('',#25133,#14415,#14416);
#12421=AXIS2_PLACEMENT_3D('',#25134,#14417,#14418);
#12422=AXIS2_PLACEMENT_3D('',#25201,#14419,#14420);
#12423=AXIS2_PLACEMENT_3D('',#25202,#14421,#14422);
#12424=AXIS2_PLACEMENT_3D('',#25203,#14423,#14424);
#12425=AXIS2_PLACEMENT_3D('',#25204,#14425,#14426);
#12426=AXIS2_PLACEMENT_3D('',#25206,#14427,#14428);
#12427=AXIS2_PLACEMENT_3D('',#25210,#14430,#14431);
#12428=AXIS2_PLACEMENT_3D('',#25211,#14432,#14433);
#12429=AXIS2_PLACEMENT_3D('',#25212,#14434,#14435);
#12430=AXIS2_PLACEMENT_3D('',#25215,#14436,#14437);
#12431=AXIS2_PLACEMENT_3D('',#25216,#14438,#14439);
#12432=AXIS2_PLACEMENT_3D('',#25219,#14441,#14442);
#12433=AXIS2_PLACEMENT_3D('',#25220,#14443,#14444);
#12434=AXIS2_PLACEMENT_3D('',#25223,#14445,#14446);
#12435=AXIS2_PLACEMENT_3D('',#25224,#14447,#14448);
#12436=AXIS2_PLACEMENT_3D('',#25227,#14450,#14451);
#12437=AXIS2_PLACEMENT_3D('',#25228,#14452,#14453);
#12438=AXIS2_PLACEMENT_3D('',#25231,#14454,#14455);
#12439=AXIS2_PLACEMENT_3D('',#25235,#14457,#14458);
#12440=AXIS2_PLACEMENT_3D('',#25237,#14460,#14461);
#12441=AXIS2_PLACEMENT_3D('',#25239,#14462,#14463);
#12442=AXIS2_PLACEMENT_3D('',#25243,#14465,#14466);
#12443=AXIS2_PLACEMENT_3D('',#25245,#14467,#14468);
#12444=AXIS2_PLACEMENT_3D('',#25247,#14469,#14470);
#12445=AXIS2_PLACEMENT_3D('',#25249,#14471,#14472);
#12446=AXIS2_PLACEMENT_3D('',#25251,#14473,#14474);
#12447=AXIS2_PLACEMENT_3D('',#25253,#14475,#14476);
#12448=AXIS2_PLACEMENT_3D('',#25255,#14477,#14478);
#12449=AXIS2_PLACEMENT_3D('',#25257,#14479,#14480);
#12450=AXIS2_PLACEMENT_3D('',#25259,#14481,#14482);
#12451=AXIS2_PLACEMENT_3D('',#25261,#14483,#14484);
#12452=AXIS2_PLACEMENT_3D('',#25263,#14485,#14486);
#12453=AXIS2_PLACEMENT_3D('',#25265,#14487,#14488);
#12454=AXIS2_PLACEMENT_3D('',#25267,#14489,#14490);
#12455=AXIS2_PLACEMENT_3D('',#25269,#14491,#14492);
#12456=AXIS2_PLACEMENT_3D('',#25271,#14493,#14494);
#12457=AXIS2_PLACEMENT_3D('',#25273,#14495,#14496);
#12458=AXIS2_PLACEMENT_3D('',#25275,#14497,#14498);
#12459=AXIS2_PLACEMENT_3D('',#25277,#14499,#14500);
#12460=AXIS2_PLACEMENT_3D('',#25279,#14501,#14502);
#12461=AXIS2_PLACEMENT_3D('',#25281,#14503,#14504);
#12462=AXIS2_PLACEMENT_3D('',#25282,#14505,#14506);
#12463=AXIS2_PLACEMENT_3D('',#25283,#14507,#14508);
#12464=AXIS2_PLACEMENT_3D('',#25285,#14509,#14510);
#12465=AXIS2_PLACEMENT_3D('',#25289,#14512,#14513);
#12466=AXIS2_PLACEMENT_3D('',#25293,#14515,#14516);
#12467=AXIS2_PLACEMENT_3D('',#25296,#14518,#14519);
#12468=AXIS2_PLACEMENT_3D('',#25298,#14520,#14521);
#12469=AXIS2_PLACEMENT_3D('',#25301,#14523,#14524);
#12470=AXIS2_PLACEMENT_3D('',#25304,#14525,#14526);
#12471=AXIS2_PLACEMENT_3D('',#25308,#14528,#14529);
#12472=AXIS2_PLACEMENT_3D('',#25314,#14532,#14533);
#12473=AXIS2_PLACEMENT_3D('',#25317,#14535,#14536);
#12474=AXIS2_PLACEMENT_3D('',#25322,#14538,#14539);
#12475=AXIS2_PLACEMENT_3D('',#25325,#14541,#14542);
#12476=AXIS2_PLACEMENT_3D('',#25330,#14544,#14545);
#12477=AXIS2_PLACEMENT_3D('',#25333,#14547,#14548);
#12478=AXIS2_PLACEMENT_3D('',#25338,#14550,#14551);
#12479=AXIS2_PLACEMENT_3D('',#25341,#14553,#14554);
#12480=AXIS2_PLACEMENT_3D('',#25344,#14555,#14556);
#12481=AXIS2_PLACEMENT_3D('',#25348,#14558,#14559);
#12482=AXIS2_PLACEMENT_3D('',#25354,#14562,#14563);
#12483=AXIS2_PLACEMENT_3D('',#25357,#14565,#14566);
#12484=AXIS2_PLACEMENT_3D('',#25362,#14568,#14569);
#12485=AXIS2_PLACEMENT_3D('',#25365,#14571,#14572);
#12486=AXIS2_PLACEMENT_3D('',#25370,#14574,#14575);
#12487=AXIS2_PLACEMENT_3D('',#25373,#14577,#14578);
#12488=AXIS2_PLACEMENT_3D('',#25374,#14579,#14580);
#12489=AXIS2_PLACEMENT_3D('',#25376,#14582,#14583);
#12490=AXIS2_PLACEMENT_3D('',#25379,#14585,#14586);
#12491=AXIS2_PLACEMENT_3D('',#25380,#14587,#14588);
#12492=AXIS2_PLACEMENT_3D('',#25386,#14592,#14593);
#12493=AXIS2_PLACEMENT_3D('',#25392,#14597,#14598);
#12494=AXIS2_PLACEMENT_3D('',#25398,#14602,#14603);
#12495=AXIS2_PLACEMENT_3D('',#25404,#14607,#14608);
#12496=AXIS2_PLACEMENT_3D('',#25410,#14612,#14613);
#12497=AXIS2_PLACEMENT_3D('',#25416,#14617,#14618);
#12498=AXIS2_PLACEMENT_3D('',#25422,#14622,#14623);
#12499=AXIS2_PLACEMENT_3D('',#25428,#14627,#14628);
#12500=AXIS2_PLACEMENT_3D('',#25434,#14632,#14633);
#12501=AXIS2_PLACEMENT_3D('',#25440,#14637,#14638);
#12502=AXIS2_PLACEMENT_3D('',#25444,#14640,#14641);
#12503=AXIS2_PLACEMENT_3D('',#25453,#14646,#14647);
#12504=AXIS2_PLACEMENT_3D('',#25462,#14652,#14653);
#12505=AXIS2_PLACEMENT_3D('',#25471,#14658,#14659);
#12506=AXIS2_PLACEMENT_3D('',#25480,#14664,#14665);
#12507=AXIS2_PLACEMENT_3D('',#25489,#14670,#14671);
#12508=AXIS2_PLACEMENT_3D('',#25498,#14676,#14677);
#12509=AXIS2_PLACEMENT_3D('',#25507,#14682,#14683);
#12510=AXIS2_PLACEMENT_3D('',#25516,#14688,#14689);
#12511=AXIS2_PLACEMENT_3D('',#25525,#14694,#14695);
#12512=AXIS2_PLACEMENT_3D('',#25536,#14702,#14703);
#12513=AXIS2_PLACEMENT_3D('',#25542,#14707,#14708);
#12514=AXIS2_PLACEMENT_3D('',#25543,#14709,#14710);
#12515=AXIS2_PLACEMENT_3D('',#25544,#14711,#14712);
#12516=AXIS2_PLACEMENT_3D('',#25550,#14716,#14717);
#12517=AXIS2_PLACEMENT_3D('',#25551,#14718,#14719);
#12518=AXIS2_PLACEMENT_3D('',#25555,#14722,#14723);
#12519=AXIS2_PLACEMENT_3D('',#25558,#14725,#14726);
#12520=AXIS2_PLACEMENT_3D('',#25559,#14727,#14728);
#12521=AXIS2_PLACEMENT_3D('',#25561,#14730,#14731);
#12522=AXIS2_PLACEMENT_3D('',#25562,#14732,#14733);
#12523=AXIS2_PLACEMENT_3D('',#25564,#14735,#14736);
#12524=AXIS2_PLACEMENT_3D('',#25565,#14737,#14738);
#12525=AXIS2_PLACEMENT_3D('',#25571,#14742,#14743);
#12526=AXIS2_PLACEMENT_3D('',#25572,#14744,#14745);
#12527=AXIS2_PLACEMENT_3D('',#25576,#14748,#14749);
#12528=AXIS2_PLACEMENT_3D('',#25579,#14751,#14752);
#12529=AXIS2_PLACEMENT_3D('',#25580,#14753,#14754);
#12530=AXIS2_PLACEMENT_3D('',#25582,#14756,#14757);
#12531=AXIS2_PLACEMENT_3D('',#25583,#14758,#14759);
#12532=AXIS2_PLACEMENT_3D('',#25585,#14761,#14762);
#12533=AXIS2_PLACEMENT_3D('',#25591,#14766,#14767);
#12534=AXIS2_PLACEMENT_3D('',#25592,#14768,#14769);
#12535=AXIS2_PLACEMENT_3D('',#25596,#14772,#14773);
#12536=AXIS2_PLACEMENT_3D('',#25599,#14775,#14776);
#12537=AXIS2_PLACEMENT_3D('',#25600,#14777,#14778);
#12538=AXIS2_PLACEMENT_3D('',#25602,#14780,#14781);
#12539=AXIS2_PLACEMENT_3D('',#25603,#14782,#14783);
#12540=AXIS2_PLACEMENT_3D('',#25605,#14785,#14786);
#12541=AXIS2_PLACEMENT_3D('',#25611,#14790,#14791);
#12542=AXIS2_PLACEMENT_3D('',#25612,#14792,#14793);
#12543=AXIS2_PLACEMENT_3D('',#25616,#14796,#14797);
#12544=AXIS2_PLACEMENT_3D('',#25619,#14799,#14800);
#12545=AXIS2_PLACEMENT_3D('',#25620,#14801,#14802);
#12546=AXIS2_PLACEMENT_3D('',#25622,#14804,#14805);
#12547=AXIS2_PLACEMENT_3D('',#25623,#14806,#14807);
#12548=AXIS2_PLACEMENT_3D('',#25625,#14809,#14810);
#12549=AXIS2_PLACEMENT_3D('',#25631,#14814,#14815);
#12550=AXIS2_PLACEMENT_3D('',#25632,#14816,#14817);
#12551=AXIS2_PLACEMENT_3D('',#25636,#14820,#14821);
#12552=AXIS2_PLACEMENT_3D('',#25639,#14823,#14824);
#12553=AXIS2_PLACEMENT_3D('',#25640,#14825,#14826);
#12554=AXIS2_PLACEMENT_3D('',#25642,#14828,#14829);
#12555=AXIS2_PLACEMENT_3D('',#25643,#14830,#14831);
#12556=AXIS2_PLACEMENT_3D('',#25645,#14833,#14834);
#12557=AXIS2_PLACEMENT_3D('',#25651,#14838,#14839);
#12558=AXIS2_PLACEMENT_3D('',#25652,#14840,#14841);
#12559=AXIS2_PLACEMENT_3D('',#25656,#14844,#14845);
#12560=AXIS2_PLACEMENT_3D('',#25659,#14847,#14848);
#12561=AXIS2_PLACEMENT_3D('',#25660,#14849,#14850);
#12562=AXIS2_PLACEMENT_3D('',#25662,#14852,#14853);
#12563=AXIS2_PLACEMENT_3D('',#25663,#14854,#14855);
#12564=AXIS2_PLACEMENT_3D('',#25665,#14857,#14858);
#12565=AXIS2_PLACEMENT_3D('',#25671,#14862,#14863);
#12566=AXIS2_PLACEMENT_3D('',#25672,#14864,#14865);
#12567=AXIS2_PLACEMENT_3D('',#25676,#14868,#14869);
#12568=AXIS2_PLACEMENT_3D('',#25679,#14871,#14872);
#12569=AXIS2_PLACEMENT_3D('',#25680,#14873,#14874);
#12570=AXIS2_PLACEMENT_3D('',#25682,#14876,#14877);
#12571=AXIS2_PLACEMENT_3D('',#25683,#14878,#14879);
#12572=AXIS2_PLACEMENT_3D('',#25685,#14881,#14882);
#12573=AXIS2_PLACEMENT_3D('',#25691,#14886,#14887);
#12574=AXIS2_PLACEMENT_3D('',#25692,#14888,#14889);
#12575=AXIS2_PLACEMENT_3D('',#25696,#14892,#14893);
#12576=AXIS2_PLACEMENT_3D('',#25699,#14895,#14896);
#12577=AXIS2_PLACEMENT_3D('',#25700,#14897,#14898);
#12578=AXIS2_PLACEMENT_3D('',#25702,#14900,#14901);
#12579=AXIS2_PLACEMENT_3D('',#25703,#14902,#14903);
#12580=AXIS2_PLACEMENT_3D('',#25705,#14905,#14906);
#12581=AXIS2_PLACEMENT_3D('',#25711,#14910,#14911);
#12582=AXIS2_PLACEMENT_3D('',#25712,#14912,#14913);
#12583=AXIS2_PLACEMENT_3D('',#25716,#14916,#14917);
#12584=AXIS2_PLACEMENT_3D('',#25719,#14919,#14920);
#12585=AXIS2_PLACEMENT_3D('',#25720,#14921,#14922);
#12586=AXIS2_PLACEMENT_3D('',#25722,#14924,#14925);
#12587=AXIS2_PLACEMENT_3D('',#25723,#14926,#14927);
#12588=AXIS2_PLACEMENT_3D('',#25725,#14929,#14930);
#12589=AXIS2_PLACEMENT_3D('',#25731,#14934,#14935);
#12590=AXIS2_PLACEMENT_3D('',#25732,#14936,#14937);
#12591=AXIS2_PLACEMENT_3D('',#25736,#14940,#14941);
#12592=AXIS2_PLACEMENT_3D('',#25739,#14943,#14944);
#12593=AXIS2_PLACEMENT_3D('',#25740,#14945,#14946);
#12594=AXIS2_PLACEMENT_3D('',#25742,#14948,#14949);
#12595=AXIS2_PLACEMENT_3D('',#25743,#14950,#14951);
#12596=AXIS2_PLACEMENT_3D('',#25745,#14953,#14954);
#12597=AXIS2_PLACEMENT_3D('',#25746,#14955,#14956);
#12598=AXIS2_PLACEMENT_3D('',#25747,#14957,#14958);
#12599=AXIS2_PLACEMENT_3D('',#25748,#14959,#14960);
#12600=AXIS2_PLACEMENT_3D('',#25749,#14961,#14962);
#12601=AXIS2_PLACEMENT_3D('',#25750,#14963,#14964);
#12602=AXIS2_PLACEMENT_3D('',#25751,#14965,#14966);
#12603=AXIS2_PLACEMENT_3D('',#25752,#14967,#14968);
#12604=AXIS2_PLACEMENT_3D('',#25753,#14969,#14970);
#12605=AXIS2_PLACEMENT_3D('',#25754,#14971,#14972);
#12606=AXIS2_PLACEMENT_3D('',#25755,#14973,#14974);
#12607=AXIS2_PLACEMENT_3D('',#25756,#14975,#14976);
#12608=AXIS2_PLACEMENT_3D('',#25757,#14977,#14978);
#12609=AXIS2_PLACEMENT_3D('',#25758,#14979,#14980);
#12610=AXIS2_PLACEMENT_3D('',#25759,#14981,#14982);
#12611=AXIS2_PLACEMENT_3D('',#25760,#14983,#14984);
#12612=AXIS2_PLACEMENT_3D('',#25761,#14985,#14986);
#12613=AXIS2_PLACEMENT_3D('',#25762,#14987,#14988);
#12614=AXIS2_PLACEMENT_3D('',#25763,#14989,#14990);
#12615=AXIS2_PLACEMENT_3D('',#25764,#14991,#14992);
#12616=AXIS2_PLACEMENT_3D('',#25765,#14993,#14994);
#12617=AXIS2_PLACEMENT_3D('',#25767,#14996,#14997);
#12618=AXIS2_PLACEMENT_3D('',#25769,#14999,#15000);
#12619=AXIS2_PLACEMENT_3D('',#25770,#15001,#15002);
#12620=AXIS2_PLACEMENT_3D('',#25771,#15003,#15004);
#12621=AXIS2_PLACEMENT_3D('',#25773,#15005,#15006);
#12622=AXIS2_PLACEMENT_3D('',#25775,#15007,#15008);
#12623=AXIS2_PLACEMENT_3D('',#25777,#15009,#15010);
#12624=AXIS2_PLACEMENT_3D('',#25778,#15011,#15012);
#12625=AXIS2_PLACEMENT_3D('',#25779,#15013,#15014);
#12626=AXIS2_PLACEMENT_3D('',#25782,#15015,#15016);
#12627=AXIS2_PLACEMENT_3D('',#25783,#15017,#15018);
#12628=AXIS2_PLACEMENT_3D('',#25785,#15019,#15020);
#12629=AXIS2_PLACEMENT_3D('',#25786,#15021,#15022);
#12630=AXIS2_PLACEMENT_3D('',#25787,#15023,#15024);
#12631=AXIS2_PLACEMENT_3D('',#25789,#15025,#15026);
#12632=AXIS2_PLACEMENT_3D('',#25792,#15028,#15029);
#12633=AXIS2_PLACEMENT_3D('',#25793,#15030,#15031);
#12634=AXIS2_PLACEMENT_3D('',#25795,#15032,#15033);
#12635=AXIS2_PLACEMENT_3D('',#25797,#15035,#15036);
#12636=AXIS2_PLACEMENT_3D('',#25799,#15037,#15038);
#12637=AXIS2_PLACEMENT_3D('',#25802,#15040,#15041);
#12638=AXIS2_PLACEMENT_3D('',#25803,#15042,#15043);
#12639=AXIS2_PLACEMENT_3D('',#25805,#15044,#15045);
#12640=AXIS2_PLACEMENT_3D('',#25807,#15047,#15048);
#12641=AXIS2_PLACEMENT_3D('',#25809,#15049,#15050);
#12642=AXIS2_PLACEMENT_3D('',#25812,#15052,#15053);
#12643=AXIS2_PLACEMENT_3D('',#25813,#15054,#15055);
#12644=AXIS2_PLACEMENT_3D('',#25815,#15056,#15057);
#12645=AXIS2_PLACEMENT_3D('',#25817,#15059,#15060);
#12646=AXIS2_PLACEMENT_3D('',#25819,#15061,#15062);
#12647=AXIS2_PLACEMENT_3D('',#25822,#15064,#15065);
#12648=AXIS2_PLACEMENT_3D('',#25823,#15066,#15067);
#12649=AXIS2_PLACEMENT_3D('',#25825,#15068,#15069);
#12650=AXIS2_PLACEMENT_3D('',#25827,#15071,#15072);
#12651=AXIS2_PLACEMENT_3D('',#25829,#15073,#15074);
#12652=AXIS2_PLACEMENT_3D('',#25832,#15076,#15077);
#12653=AXIS2_PLACEMENT_3D('',#25833,#15078,#15079);
#12654=AXIS2_PLACEMENT_3D('',#25835,#15080,#15081);
#12655=AXIS2_PLACEMENT_3D('',#25837,#15083,#15084);
#12656=AXIS2_PLACEMENT_3D('',#25839,#15085,#15086);
#12657=AXIS2_PLACEMENT_3D('',#25842,#15088,#15089);
#12658=AXIS2_PLACEMENT_3D('',#25843,#15090,#15091);
#12659=AXIS2_PLACEMENT_3D('',#25845,#15092,#15093);
#12660=AXIS2_PLACEMENT_3D('',#25847,#15095,#15096);
#12661=AXIS2_PLACEMENT_3D('',#25849,#15097,#15098);
#12662=AXIS2_PLACEMENT_3D('',#25852,#15100,#15101);
#12663=AXIS2_PLACEMENT_3D('',#25853,#15102,#15103);
#12664=AXIS2_PLACEMENT_3D('',#25855,#15105,#15106);
#12665=AXIS2_PLACEMENT_3D('',#25856,#15107,#15108);
#12666=AXIS2_PLACEMENT_3D('',#25857,#15109,#15110);
#12667=AXIS2_PLACEMENT_3D('',#25858,#15111,#15112);
#12668=AXIS2_PLACEMENT_3D('',#25867,#15117,#15118);
#12669=AXIS2_PLACEMENT_3D('',#25873,#15122,#15123);
#12670=AXIS2_PLACEMENT_3D('',#25875,#15124,#15125);
#12671=AXIS2_PLACEMENT_3D('',#25878,#15127,#15128);
#12672=AXIS2_PLACEMENT_3D('',#25879,#15129,#15130);
#12673=AXIS2_PLACEMENT_3D('',#25885,#15134,#15135);
#12674=AXIS2_PLACEMENT_3D('',#25887,#15136,#15137);
#12675=AXIS2_PLACEMENT_3D('',#25890,#15139,#15140);
#12676=AXIS2_PLACEMENT_3D('',#25891,#15141,#15142);
#12677=AXIS2_PLACEMENT_3D('',#25897,#15146,#15147);
#12678=AXIS2_PLACEMENT_3D('',#25899,#15148,#15149);
#12679=AXIS2_PLACEMENT_3D('',#25902,#15151,#15152);
#12680=AXIS2_PLACEMENT_3D('',#25903,#15153,#15154);
#12681=AXIS2_PLACEMENT_3D('',#25909,#15158,#15159);
#12682=AXIS2_PLACEMENT_3D('',#25911,#15160,#15161);
#12683=AXIS2_PLACEMENT_3D('',#25914,#15163,#15164);
#12684=AXIS2_PLACEMENT_3D('',#25915,#15165,#15166);
#12685=AXIS2_PLACEMENT_3D('',#25921,#15170,#15171);
#12686=AXIS2_PLACEMENT_3D('',#25927,#15175,#15176);
#12687=AXIS2_PLACEMENT_3D('',#25930,#15179,#15180);
#12688=AXIS2_PLACEMENT_3D('',#25931,#15181,#15182);
#12689=AXIS2_PLACEMENT_3D('',#25932,#15183,#15184);
#12690=AXIS2_PLACEMENT_3D('',#25937,#15186,#15187);
#12691=AXIS2_PLACEMENT_3D('',#25941,#15189,#15190);
#12692=AXIS2_PLACEMENT_3D('',#25945,#15192,#15193);
#12693=AXIS2_PLACEMENT_3D('',#25949,#15195,#15196);
#12694=AXIS2_PLACEMENT_3D('',#25957,#15201,#15202);
#12695=AXIS2_PLACEMENT_3D('',#25963,#15206,#15207);
#12696=AXIS2_PLACEMENT_3D('',#25967,#15210,#15211);
#12697=AXIS2_PLACEMENT_3D('',#25971,#15214,#15215);
#12698=AXIS2_PLACEMENT_3D('',#25974,#15217,#15218);
#12699=AXIS2_PLACEMENT_3D('',#25975,#15219,#15220);
#12700=AXIS2_PLACEMENT_3D('',#25979,#15223,#15224);
#12701=AXIS2_PLACEMENT_3D('',#25982,#15226,#15227);
#12702=AXIS2_PLACEMENT_3D('',#25983,#15228,#15229);
#12703=AXIS2_PLACEMENT_3D('',#25987,#15232,#15233);
#12704=AXIS2_PLACEMENT_3D('',#25990,#15235,#15236);
#12705=AXIS2_PLACEMENT_3D('',#25991,#15237,#15238);
#12706=AXIS2_PLACEMENT_3D('',#25995,#15241,#15242);
#12707=AXIS2_PLACEMENT_3D('',#25998,#15244,#15245);
#12708=AXIS2_PLACEMENT_3D('',#25999,#15246,#15247);
#12709=AXIS2_PLACEMENT_3D('',#26003,#15250,#15251);
#12710=AXIS2_PLACEMENT_3D('',#26005,#15253,#15254);
#12711=AXIS2_PLACEMENT_3D('',#26006,#15255,#15256);
#12712=AXIS2_PLACEMENT_3D('',#26019,#15262,#15263);
#12713=AXIS2_PLACEMENT_3D('',#26023,#15265,#15266);
#12714=AXIS2_PLACEMENT_3D('',#26027,#15268,#15269);
#12715=AXIS2_PLACEMENT_3D('',#26030,#15271,#15272);
#12716=AXIS2_PLACEMENT_3D('',#26031,#15273,#15274);
#12717=AXIS2_PLACEMENT_3D('',#26037,#15278,#15279);
#12718=AXIS2_PLACEMENT_3D('',#26041,#15282,#15283);
#12719=AXIS2_PLACEMENT_3D('',#26045,#15286,#15287);
#12720=AXIS2_PLACEMENT_3D('',#26047,#15288,#15289);
#12721=AXIS2_PLACEMENT_3D('',#26049,#15291,#15292);
#12722=AXIS2_PLACEMENT_3D('',#26053,#15295,#15296);
#12723=AXIS2_PLACEMENT_3D('',#26055,#15297,#15298);
#12724=AXIS2_PLACEMENT_3D('',#26057,#15300,#15301);
#12725=AXIS2_PLACEMENT_3D('',#26061,#15304,#15305);
#12726=AXIS2_PLACEMENT_3D('',#26063,#15306,#15307);
#12727=AXIS2_PLACEMENT_3D('',#26065,#15309,#15310);
#12728=AXIS2_PLACEMENT_3D('',#26069,#15313,#15314);
#12729=AXIS2_PLACEMENT_3D('',#26071,#15315,#15316);
#12730=AXIS2_PLACEMENT_3D('',#26073,#15318,#15319);
#12731=AXIS2_PLACEMENT_3D('',#26077,#15322,#15323);
#12732=AXIS2_PLACEMENT_3D('',#26079,#15325,#15326);
#12733=AXIS2_PLACEMENT_3D('',#26080,#15327,#15328);
#12734=AXIS2_PLACEMENT_3D('',#26089,#15333,#15334);
#12735=AXIS2_PLACEMENT_3D('',#26095,#15338,#15339);
#12736=AXIS2_PLACEMENT_3D('',#26097,#15340,#15341);
#12737=AXIS2_PLACEMENT_3D('',#26099,#15342,#15343);
#12738=AXIS2_PLACEMENT_3D('',#26101,#15345,#15346);
#12739=AXIS2_PLACEMENT_3D('',#26107,#15350,#15351);
#12740=AXIS2_PLACEMENT_3D('',#26109,#15352,#15353);
#12741=AXIS2_PLACEMENT_3D('',#26111,#15354,#15355);
#12742=AXIS2_PLACEMENT_3D('',#26113,#15357,#15358);
#12743=AXIS2_PLACEMENT_3D('',#26119,#15362,#15363);
#12744=AXIS2_PLACEMENT_3D('',#26121,#15364,#15365);
#12745=AXIS2_PLACEMENT_3D('',#26123,#15366,#15367);
#12746=AXIS2_PLACEMENT_3D('',#26125,#15369,#15370);
#12747=AXIS2_PLACEMENT_3D('',#26131,#15374,#15375);
#12748=AXIS2_PLACEMENT_3D('',#26133,#15376,#15377);
#12749=AXIS2_PLACEMENT_3D('',#26135,#15378,#15379);
#12750=AXIS2_PLACEMENT_3D('',#26137,#15381,#15382);
#12751=AXIS2_PLACEMENT_3D('',#26143,#15386,#15387);
#12752=AXIS2_PLACEMENT_3D('',#26149,#15391,#15392);
#12753=AXIS2_PLACEMENT_3D('',#26152,#15395,#15396);
#12754=AXIS2_PLACEMENT_3D('',#26153,#15397,#15398);
#12755=AXIS2_PLACEMENT_3D('',#26154,#15399,#15400);
#12756=AXIS2_PLACEMENT_3D('',#26163,#15405,#15406);
#12757=AXIS2_PLACEMENT_3D('',#26169,#15410,#15411);
#12758=AXIS2_PLACEMENT_3D('',#26171,#15412,#15413);
#12759=AXIS2_PLACEMENT_3D('',#26174,#15415,#15416);
#12760=AXIS2_PLACEMENT_3D('',#26175,#15417,#15418);
#12761=AXIS2_PLACEMENT_3D('',#26181,#15422,#15423);
#12762=AXIS2_PLACEMENT_3D('',#26183,#15424,#15425);
#12763=AXIS2_PLACEMENT_3D('',#26186,#15427,#15428);
#12764=AXIS2_PLACEMENT_3D('',#26187,#15429,#15430);
#12765=AXIS2_PLACEMENT_3D('',#26193,#15434,#15435);
#12766=AXIS2_PLACEMENT_3D('',#26195,#15436,#15437);
#12767=AXIS2_PLACEMENT_3D('',#26198,#15439,#15440);
#12768=AXIS2_PLACEMENT_3D('',#26199,#15441,#15442);
#12769=AXIS2_PLACEMENT_3D('',#26205,#15446,#15447);
#12770=AXIS2_PLACEMENT_3D('',#26207,#15448,#15449);
#12771=AXIS2_PLACEMENT_3D('',#26210,#15451,#15452);
#12772=AXIS2_PLACEMENT_3D('',#26211,#15453,#15454);
#12773=AXIS2_PLACEMENT_3D('',#26217,#15458,#15459);
#12774=AXIS2_PLACEMENT_3D('',#26223,#15463,#15464);
#12775=AXIS2_PLACEMENT_3D('',#26226,#15467,#15468);
#12776=AXIS2_PLACEMENT_3D('',#26227,#15469,#15470);
#12777=AXIS2_PLACEMENT_3D('',#26228,#15471,#15472);
#12778=AXIS2_PLACEMENT_3D('',#26241,#15478,#15479);
#12779=AXIS2_PLACEMENT_3D('',#26245,#15481,#15482);
#12780=AXIS2_PLACEMENT_3D('',#26249,#15484,#15485);
#12781=AXIS2_PLACEMENT_3D('',#26252,#15487,#15488);
#12782=AXIS2_PLACEMENT_3D('',#26253,#15489,#15490);
#12783=AXIS2_PLACEMENT_3D('',#26259,#15494,#15495);
#12784=AXIS2_PLACEMENT_3D('',#26263,#15498,#15499);
#12785=AXIS2_PLACEMENT_3D('',#26267,#15502,#15503);
#12786=AXIS2_PLACEMENT_3D('',#26269,#15504,#15505);
#12787=AXIS2_PLACEMENT_3D('',#26271,#15507,#15508);
#12788=AXIS2_PLACEMENT_3D('',#26275,#15511,#15512);
#12789=AXIS2_PLACEMENT_3D('',#26277,#15513,#15514);
#12790=AXIS2_PLACEMENT_3D('',#26279,#15516,#15517);
#12791=AXIS2_PLACEMENT_3D('',#26283,#15520,#15521);
#12792=AXIS2_PLACEMENT_3D('',#26285,#15522,#15523);
#12793=AXIS2_PLACEMENT_3D('',#26287,#15525,#15526);
#12794=AXIS2_PLACEMENT_3D('',#26291,#15529,#15530);
#12795=AXIS2_PLACEMENT_3D('',#26293,#15531,#15532);
#12796=AXIS2_PLACEMENT_3D('',#26295,#15534,#15535);
#12797=AXIS2_PLACEMENT_3D('',#26299,#15538,#15539);
#12798=AXIS2_PLACEMENT_3D('',#26301,#15541,#15542);
#12799=AXIS2_PLACEMENT_3D('',#26302,#15543,#15544);
#12800=AXIS2_PLACEMENT_3D('',#26311,#15549,#15550);
#12801=AXIS2_PLACEMENT_3D('',#26317,#15554,#15555);
#12802=AXIS2_PLACEMENT_3D('',#26319,#15556,#15557);
#12803=AXIS2_PLACEMENT_3D('',#26322,#15559,#15560);
#12804=AXIS2_PLACEMENT_3D('',#26323,#15561,#15562);
#12805=AXIS2_PLACEMENT_3D('',#26329,#15566,#15567);
#12806=AXIS2_PLACEMENT_3D('',#26331,#15568,#15569);
#12807=AXIS2_PLACEMENT_3D('',#26334,#15571,#15572);
#12808=AXIS2_PLACEMENT_3D('',#26335,#15573,#15574);
#12809=AXIS2_PLACEMENT_3D('',#26341,#15578,#15579);
#12810=AXIS2_PLACEMENT_3D('',#26343,#15580,#15581);
#12811=AXIS2_PLACEMENT_3D('',#26346,#15583,#15584);
#12812=AXIS2_PLACEMENT_3D('',#26347,#15585,#15586);
#12813=AXIS2_PLACEMENT_3D('',#26353,#15590,#15591);
#12814=AXIS2_PLACEMENT_3D('',#26355,#15592,#15593);
#12815=AXIS2_PLACEMENT_3D('',#26358,#15595,#15596);
#12816=AXIS2_PLACEMENT_3D('',#26359,#15597,#15598);
#12817=AXIS2_PLACEMENT_3D('',#26365,#15602,#15603);
#12818=AXIS2_PLACEMENT_3D('',#26371,#15607,#15608);
#12819=AXIS2_PLACEMENT_3D('',#26374,#15611,#15612);
#12820=AXIS2_PLACEMENT_3D('',#26375,#15613,#15614);
#12821=AXIS2_PLACEMENT_3D('',#26376,#15615,#15616);
#12822=AXIS2_PLACEMENT_3D('',#26389,#15622,#15623);
#12823=AXIS2_PLACEMENT_3D('',#26393,#15625,#15626);
#12824=AXIS2_PLACEMENT_3D('',#26397,#15628,#15629);
#12825=AXIS2_PLACEMENT_3D('',#26400,#15631,#15632);
#12826=AXIS2_PLACEMENT_3D('',#26401,#15633,#15634);
#12827=AXIS2_PLACEMENT_3D('',#26407,#15638,#15639);
#12828=AXIS2_PLACEMENT_3D('',#26411,#15642,#15643);
#12829=AXIS2_PLACEMENT_3D('',#26415,#15646,#15647);
#12830=AXIS2_PLACEMENT_3D('',#26417,#15648,#15649);
#12831=AXIS2_PLACEMENT_3D('',#26419,#15651,#15652);
#12832=AXIS2_PLACEMENT_3D('',#26423,#15655,#15656);
#12833=AXIS2_PLACEMENT_3D('',#26425,#15657,#15658);
#12834=AXIS2_PLACEMENT_3D('',#26427,#15660,#15661);
#12835=AXIS2_PLACEMENT_3D('',#26431,#15664,#15665);
#12836=AXIS2_PLACEMENT_3D('',#26433,#15666,#15667);
#12837=AXIS2_PLACEMENT_3D('',#26435,#15669,#15670);
#12838=AXIS2_PLACEMENT_3D('',#26439,#15673,#15674);
#12839=AXIS2_PLACEMENT_3D('',#26441,#15675,#15676);
#12840=AXIS2_PLACEMENT_3D('',#26443,#15678,#15679);
#12841=AXIS2_PLACEMENT_3D('',#26447,#15682,#15683);
#12842=AXIS2_PLACEMENT_3D('',#26449,#15685,#15686);
#12843=AXIS2_PLACEMENT_3D('',#26450,#15687,#15688);
#12844=AXIS2_PLACEMENT_3D('',#26457,#15691,#15692);
#12845=AXIS2_PLACEMENT_3D('',#26461,#15694,#15695);
#12846=AXIS2_PLACEMENT_3D('',#26465,#15697,#15698);
#12847=AXIS2_PLACEMENT_3D('',#26469,#15700,#15701);
#12848=AXIS2_PLACEMENT_3D('',#26475,#15705,#15706);
#12849=AXIS2_PLACEMENT_3D('',#26481,#15710,#15711);
#12850=AXIS2_PLACEMENT_3D('',#26485,#15714,#15715);
#12851=AXIS2_PLACEMENT_3D('',#26489,#15718,#15719);
#12852=AXIS2_PLACEMENT_3D('',#26492,#15721,#15722);
#12853=AXIS2_PLACEMENT_3D('',#26493,#15723,#15724);
#12854=AXIS2_PLACEMENT_3D('',#26497,#15727,#15728);
#12855=AXIS2_PLACEMENT_3D('',#26500,#15730,#15731);
#12856=AXIS2_PLACEMENT_3D('',#26501,#15732,#15733);
#12857=AXIS2_PLACEMENT_3D('',#26505,#15736,#15737);
#12858=AXIS2_PLACEMENT_3D('',#26508,#15739,#15740);
#12859=AXIS2_PLACEMENT_3D('',#26509,#15741,#15742);
#12860=AXIS2_PLACEMENT_3D('',#26513,#15745,#15746);
#12861=AXIS2_PLACEMENT_3D('',#26516,#15748,#15749);
#12862=AXIS2_PLACEMENT_3D('',#26517,#15750,#15751);
#12863=AXIS2_PLACEMENT_3D('',#26521,#15754,#15755);
#12864=AXIS2_PLACEMENT_3D('',#26523,#15757,#15758);
#12865=AXIS2_PLACEMENT_3D('',#26524,#15759,#15760);
#12866=AXIS2_PLACEMENT_3D('',#26535,#15765,#15766);
#12867=AXIS2_PLACEMENT_3D('',#26539,#15768,#15769);
#12868=AXIS2_PLACEMENT_3D('',#26543,#15771,#15772);
#12869=AXIS2_PLACEMENT_3D('',#26547,#15774,#15775);
#12870=AXIS2_PLACEMENT_3D('',#26549,#15777,#15778);
#12871=AXIS2_PLACEMENT_3D('',#26555,#15782,#15783);
#12872=AXIS2_PLACEMENT_3D('',#26559,#15786,#15787);
#12873=AXIS2_PLACEMENT_3D('',#26563,#15790,#15791);
#12874=AXIS2_PLACEMENT_3D('',#26565,#15792,#15793);
#12875=AXIS2_PLACEMENT_3D('',#26567,#15795,#15796);
#12876=AXIS2_PLACEMENT_3D('',#26571,#15799,#15800);
#12877=AXIS2_PLACEMENT_3D('',#26573,#15801,#15802);
#12878=AXIS2_PLACEMENT_3D('',#26575,#15804,#15805);
#12879=AXIS2_PLACEMENT_3D('',#26579,#15808,#15809);
#12880=AXIS2_PLACEMENT_3D('',#26581,#15810,#15811);
#12881=AXIS2_PLACEMENT_3D('',#26583,#15813,#15814);
#12882=AXIS2_PLACEMENT_3D('',#26587,#15817,#15818);
#12883=AXIS2_PLACEMENT_3D('',#26589,#15819,#15820);
#12884=AXIS2_PLACEMENT_3D('',#26591,#15822,#15823);
#12885=AXIS2_PLACEMENT_3D('',#26595,#15826,#15827);
#12886=AXIS2_PLACEMENT_3D('',#26597,#15829,#15830);
#12887=AXIS2_PLACEMENT_3D('',#26598,#15831,#15832);
#12888=AXIS2_PLACEMENT_3D('',#26607,#15837,#15838);
#12889=AXIS2_PLACEMENT_3D('',#26613,#15842,#15843);
#12890=AXIS2_PLACEMENT_3D('',#26615,#15844,#15845);
#12891=AXIS2_PLACEMENT_3D('',#26618,#15847,#15848);
#12892=AXIS2_PLACEMENT_3D('',#26619,#15849,#15850);
#12893=AXIS2_PLACEMENT_3D('',#26625,#15854,#15855);
#12894=AXIS2_PLACEMENT_3D('',#26627,#15856,#15857);
#12895=AXIS2_PLACEMENT_3D('',#26630,#15859,#15860);
#12896=AXIS2_PLACEMENT_3D('',#26631,#15861,#15862);
#12897=AXIS2_PLACEMENT_3D('',#26637,#15866,#15867);
#12898=AXIS2_PLACEMENT_3D('',#26639,#15868,#15869);
#12899=AXIS2_PLACEMENT_3D('',#26642,#15871,#15872);
#12900=AXIS2_PLACEMENT_3D('',#26643,#15873,#15874);
#12901=AXIS2_PLACEMENT_3D('',#26649,#15878,#15879);
#12902=AXIS2_PLACEMENT_3D('',#26652,#15882,#15883);
#12903=AXIS2_PLACEMENT_3D('',#26653,#15884,#15885);
#12904=AXIS2_PLACEMENT_3D('',#26654,#15886,#15887);
#12905=AXIS2_PLACEMENT_3D('',#26663,#15892,#15893);
#12906=AXIS2_PLACEMENT_3D('',#26669,#15897,#15898);
#12907=AXIS2_PLACEMENT_3D('',#26671,#15899,#15900);
#12908=AXIS2_PLACEMENT_3D('',#26674,#15902,#15903);
#12909=AXIS2_PLACEMENT_3D('',#26675,#15904,#15905);
#12910=AXIS2_PLACEMENT_3D('',#26681,#15909,#15910);
#12911=AXIS2_PLACEMENT_3D('',#26683,#15911,#15912);
#12912=AXIS2_PLACEMENT_3D('',#26686,#15914,#15915);
#12913=AXIS2_PLACEMENT_3D('',#26687,#15916,#15917);
#12914=AXIS2_PLACEMENT_3D('',#26693,#15921,#15922);
#12915=AXIS2_PLACEMENT_3D('',#26695,#15923,#15924);
#12916=AXIS2_PLACEMENT_3D('',#26698,#15926,#15927);
#12917=AXIS2_PLACEMENT_3D('',#26699,#15928,#15929);
#12918=AXIS2_PLACEMENT_3D('',#26705,#15933,#15934);
#12919=AXIS2_PLACEMENT_3D('',#26708,#15937,#15938);
#12920=AXIS2_PLACEMENT_3D('',#26709,#15939,#15940);
#12921=AXIS2_PLACEMENT_3D('',#26710,#15941,#15942);
#12922=AXIS2_PLACEMENT_3D('',#26719,#15947,#15948);
#12923=AXIS2_PLACEMENT_3D('',#26725,#15952,#15953);
#12924=AXIS2_PLACEMENT_3D('',#26727,#15954,#15955);
#12925=AXIS2_PLACEMENT_3D('',#26729,#15956,#15957);
#12926=AXIS2_PLACEMENT_3D('',#26731,#15959,#15960);
#12927=AXIS2_PLACEMENT_3D('',#26737,#15964,#15965);
#12928=AXIS2_PLACEMENT_3D('',#26739,#15966,#15967);
#12929=AXIS2_PLACEMENT_3D('',#26741,#15968,#15969);
#12930=AXIS2_PLACEMENT_3D('',#26743,#15971,#15972);
#12931=AXIS2_PLACEMENT_3D('',#26749,#15976,#15977);
#12932=AXIS2_PLACEMENT_3D('',#26751,#15978,#15979);
#12933=AXIS2_PLACEMENT_3D('',#26753,#15980,#15981);
#12934=AXIS2_PLACEMENT_3D('',#26755,#15983,#15984);
#12935=AXIS2_PLACEMENT_3D('',#26761,#15988,#15989);
#12936=AXIS2_PLACEMENT_3D('',#26764,#15992,#15993);
#12937=AXIS2_PLACEMENT_3D('',#26765,#15994,#15995);
#12938=AXIS2_PLACEMENT_3D('',#26766,#15996,#15997);
#12939=AXIS2_PLACEMENT_3D('',#26775,#16002,#16003);
#12940=AXIS2_PLACEMENT_3D('',#26781,#16007,#16008);
#12941=AXIS2_PLACEMENT_3D('',#26783,#16009,#16010);
#12942=AXIS2_PLACEMENT_3D('',#26785,#16011,#16012);
#12943=AXIS2_PLACEMENT_3D('',#26787,#16014,#16015);
#12944=AXIS2_PLACEMENT_3D('',#26793,#16019,#16020);
#12945=AXIS2_PLACEMENT_3D('',#26795,#16021,#16022);
#12946=AXIS2_PLACEMENT_3D('',#26797,#16023,#16024);
#12947=AXIS2_PLACEMENT_3D('',#26799,#16026,#16027);
#12948=AXIS2_PLACEMENT_3D('',#26805,#16031,#16032);
#12949=AXIS2_PLACEMENT_3D('',#26807,#16033,#16034);
#12950=AXIS2_PLACEMENT_3D('',#26809,#16035,#16036);
#12951=AXIS2_PLACEMENT_3D('',#26811,#16038,#16039);
#12952=AXIS2_PLACEMENT_3D('',#26817,#16043,#16044);
#12953=AXIS2_PLACEMENT_3D('',#26820,#16047,#16048);
#12954=AXIS2_PLACEMENT_3D('',#26821,#16049,#16050);
#12955=AXIS2_PLACEMENT_3D('',#26822,#16051,#16052);
#12956=AXIS2_PLACEMENT_3D('',#26829,#16055,#16056);
#12957=AXIS2_PLACEMENT_3D('',#26833,#16058,#16059);
#12958=AXIS2_PLACEMENT_3D('',#26837,#16061,#16062);
#12959=AXIS2_PLACEMENT_3D('',#26841,#16065,#16066);
#12960=AXIS2_PLACEMENT_3D('',#26847,#16070,#16071);
#12961=AXIS2_PLACEMENT_3D('',#26851,#16074,#16075);
#12962=AXIS2_PLACEMENT_3D('',#26854,#16077,#16078);
#12963=AXIS2_PLACEMENT_3D('',#26855,#16079,#16080);
#12964=AXIS2_PLACEMENT_3D('',#26859,#16083,#16084);
#12965=AXIS2_PLACEMENT_3D('',#26862,#16086,#16087);
#12966=AXIS2_PLACEMENT_3D('',#26863,#16088,#16089);
#12967=AXIS2_PLACEMENT_3D('',#26867,#16092,#16093);
#12968=AXIS2_PLACEMENT_3D('',#26870,#16095,#16096);
#12969=AXIS2_PLACEMENT_3D('',#26871,#16097,#16098);
#12970=AXIS2_PLACEMENT_3D('',#26875,#16101,#16102);
#12971=AXIS2_PLACEMENT_3D('',#26877,#16104,#16105);
#12972=AXIS2_PLACEMENT_3D('',#26878,#16106,#16107);
#12973=AXIS2_PLACEMENT_3D('',#26887,#16112,#16113);
#12974=AXIS2_PLACEMENT_3D('',#26893,#16117,#16118);
#12975=AXIS2_PLACEMENT_3D('',#26895,#16119,#16120);
#12976=AXIS2_PLACEMENT_3D('',#26898,#16122,#16123);
#12977=AXIS2_PLACEMENT_3D('',#26899,#16124,#16125);
#12978=AXIS2_PLACEMENT_3D('',#26905,#16129,#16130);
#12979=AXIS2_PLACEMENT_3D('',#26907,#16131,#16132);
#12980=AXIS2_PLACEMENT_3D('',#26910,#16134,#16135);
#12981=AXIS2_PLACEMENT_3D('',#26911,#16136,#16137);
#12982=AXIS2_PLACEMENT_3D('',#26917,#16141,#16142);
#12983=AXIS2_PLACEMENT_3D('',#26919,#16143,#16144);
#12984=AXIS2_PLACEMENT_3D('',#26922,#16146,#16147);
#12985=AXIS2_PLACEMENT_3D('',#26923,#16148,#16149);
#12986=AXIS2_PLACEMENT_3D('',#26929,#16153,#16154);
#12987=AXIS2_PLACEMENT_3D('',#26932,#16157,#16158);
#12988=AXIS2_PLACEMENT_3D('',#26933,#16159,#16160);
#12989=AXIS2_PLACEMENT_3D('',#26934,#16161,#16162);
#12990=AXIS2_PLACEMENT_3D('',#26943,#16166,#16167);
#12991=AXIS2_PLACEMENT_3D('',#26947,#16169,#16170);
#12992=AXIS2_PLACEMENT_3D('',#26951,#16172,#16173);
#12993=AXIS2_PLACEMENT_3D('',#26953,#16175,#16176);
#12994=AXIS2_PLACEMENT_3D('',#26959,#16180,#16181);
#12995=AXIS2_PLACEMENT_3D('',#26963,#16184,#16185);
#12996=AXIS2_PLACEMENT_3D('',#26965,#16186,#16187);
#12997=AXIS2_PLACEMENT_3D('',#26967,#16189,#16190);
#12998=AXIS2_PLACEMENT_3D('',#26971,#16193,#16194);
#12999=AXIS2_PLACEMENT_3D('',#26973,#16195,#16196);
#13000=AXIS2_PLACEMENT_3D('',#26975,#16198,#16199);
#13001=AXIS2_PLACEMENT_3D('',#26979,#16202,#16203);
#13002=AXIS2_PLACEMENT_3D('',#26981,#16204,#16205);
#13003=AXIS2_PLACEMENT_3D('',#26983,#16207,#16208);
#13004=AXIS2_PLACEMENT_3D('',#26987,#16211,#16212);
#13005=AXIS2_PLACEMENT_3D('',#26989,#16214,#16215);
#13006=AXIS2_PLACEMENT_3D('',#26990,#16216,#16217);
#13007=AXIS2_PLACEMENT_3D('',#26999,#16221,#16222);
#13008=AXIS2_PLACEMENT_3D('',#27003,#16224,#16225);
#13009=AXIS2_PLACEMENT_3D('',#27007,#16227,#16228);
#13010=AXIS2_PLACEMENT_3D('',#27009,#16230,#16231);
#13011=AXIS2_PLACEMENT_3D('',#27015,#16235,#16236);
#13012=AXIS2_PLACEMENT_3D('',#27019,#16239,#16240);
#13013=AXIS2_PLACEMENT_3D('',#27021,#16241,#16242);
#13014=AXIS2_PLACEMENT_3D('',#27023,#16244,#16245);
#13015=AXIS2_PLACEMENT_3D('',#27027,#16248,#16249);
#13016=AXIS2_PLACEMENT_3D('',#27029,#16250,#16251);
#13017=AXIS2_PLACEMENT_3D('',#27031,#16253,#16254);
#13018=AXIS2_PLACEMENT_3D('',#27035,#16257,#16258);
#13019=AXIS2_PLACEMENT_3D('',#27037,#16259,#16260);
#13020=AXIS2_PLACEMENT_3D('',#27039,#16262,#16263);
#13021=AXIS2_PLACEMENT_3D('',#27043,#16266,#16267);
#13022=AXIS2_PLACEMENT_3D('',#27045,#16269,#16270);
#13023=AXIS2_PLACEMENT_3D('',#27046,#16271,#16272);
#13024=AXIS2_PLACEMENT_3D('',#27055,#16277,#16278);
#13025=AXIS2_PLACEMENT_3D('',#27061,#16282,#16283);
#13026=AXIS2_PLACEMENT_3D('',#27063,#16284,#16285);
#13027=AXIS2_PLACEMENT_3D('',#27065,#16286,#16287);
#13028=AXIS2_PLACEMENT_3D('',#27067,#16289,#16290);
#13029=AXIS2_PLACEMENT_3D('',#27073,#16294,#16295);
#13030=AXIS2_PLACEMENT_3D('',#27075,#16296,#16297);
#13031=AXIS2_PLACEMENT_3D('',#27077,#16298,#16299);
#13032=AXIS2_PLACEMENT_3D('',#27079,#16301,#16302);
#13033=AXIS2_PLACEMENT_3D('',#27085,#16306,#16307);
#13034=AXIS2_PLACEMENT_3D('',#27087,#16308,#16309);
#13035=AXIS2_PLACEMENT_3D('',#27089,#16310,#16311);
#13036=AXIS2_PLACEMENT_3D('',#27091,#16313,#16314);
#13037=AXIS2_PLACEMENT_3D('',#27097,#16318,#16319);
#13038=AXIS2_PLACEMENT_3D('',#27100,#16322,#16323);
#13039=AXIS2_PLACEMENT_3D('',#27101,#16324,#16325);
#13040=AXIS2_PLACEMENT_3D('',#27102,#16326,#16327);
#13041=AXIS2_PLACEMENT_3D('',#27109,#16330,#16331);
#13042=AXIS2_PLACEMENT_3D('',#27113,#16333,#16334);
#13043=AXIS2_PLACEMENT_3D('',#27117,#16336,#16337);
#13044=AXIS2_PLACEMENT_3D('',#27121,#16340,#16341);
#13045=AXIS2_PLACEMENT_3D('',#27127,#16345,#16346);
#13046=AXIS2_PLACEMENT_3D('',#27131,#16349,#16350);
#13047=AXIS2_PLACEMENT_3D('',#27134,#16352,#16353);
#13048=AXIS2_PLACEMENT_3D('',#27135,#16354,#16355);
#13049=AXIS2_PLACEMENT_3D('',#27139,#16358,#16359);
#13050=AXIS2_PLACEMENT_3D('',#27142,#16361,#16362);
#13051=AXIS2_PLACEMENT_3D('',#27143,#16363,#16364);
#13052=AXIS2_PLACEMENT_3D('',#27147,#16367,#16368);
#13053=AXIS2_PLACEMENT_3D('',#27150,#16370,#16371);
#13054=AXIS2_PLACEMENT_3D('',#27151,#16372,#16373);
#13055=AXIS2_PLACEMENT_3D('',#27155,#16376,#16377);
#13056=AXIS2_PLACEMENT_3D('',#27157,#16379,#16380);
#13057=AXIS2_PLACEMENT_3D('',#27158,#16381,#16382);
#13058=AXIS2_PLACEMENT_3D('',#27161,#16383,#16384);
#13059=AXIS2_PLACEMENT_3D('',#27165,#16386,#16387);
#13060=AXIS2_PLACEMENT_3D('',#27167,#16389,#16390);
#13061=AXIS2_PLACEMENT_3D('',#27170,#16391,#16392);
#13062=AXIS2_PLACEMENT_3D('',#27174,#16394,#16395);
#13063=AXIS2_PLACEMENT_3D('',#27176,#16397,#16398);
#13064=AXIS2_PLACEMENT_3D('',#27179,#16399,#16400);
#13065=AXIS2_PLACEMENT_3D('',#27183,#16402,#16403);
#13066=AXIS2_PLACEMENT_3D('',#27185,#16405,#16406);
#13067=AXIS2_PLACEMENT_3D('',#27188,#16407,#16408);
#13068=AXIS2_PLACEMENT_3D('',#27192,#16410,#16411);
#13069=AXIS2_PLACEMENT_3D('',#27194,#16413,#16414);
#13070=AXIS2_PLACEMENT_3D('',#27203,#16419,#16420);
#13071=AXIS2_PLACEMENT_3D('',#27212,#16425,#16426);
#13072=AXIS2_PLACEMENT_3D('',#27221,#16431,#16432);
#13073=AXIS2_PLACEMENT_3D('',#27230,#16437,#16438);
#13074=AXIS2_PLACEMENT_3D('',#27239,#16445,#16446);
#13075=AXIS2_PLACEMENT_3D('',#27244,#16449,#16450);
#13076=AXIS2_PLACEMENT_3D('',#27249,#16453,#16454);
#13077=AXIS2_PLACEMENT_3D('',#27254,#16457,#16458);
#13078=AXIS2_PLACEMENT_3D('',#27255,#16459,#16460);
#13079=AXIS2_PLACEMENT_3D('',#27263,#16466,#16467);
#13080=AXIS2_PLACEMENT_3D('',#27268,#16470,#16471);
#13081=AXIS2_PLACEMENT_3D('',#27273,#16474,#16475);
#13082=AXIS2_PLACEMENT_3D('',#27278,#16478,#16479);
#13083=AXIS2_PLACEMENT_3D('',#27280,#16481,#16482);
#13084=AXIS2_PLACEMENT_3D('',#27282,#16484,#16485);
#13085=AXIS2_PLACEMENT_3D('',#27284,#16487,#16488);
#13086=AXIS2_PLACEMENT_3D('',#27285,#16489,#16490);
#13087=AXIS2_PLACEMENT_3D('',#27287,#16492,#16493);
#13088=AXIS2_PLACEMENT_3D('',#27289,#16495,#16496);
#13089=AXIS2_PLACEMENT_3D('',#27290,#16497,#16498);
#13090=AXIS2_PLACEMENT_3D('',#27292,#16500,#16501);
#13091=AXIS2_PLACEMENT_3D('',#27294,#16503,#16504);
#13092=AXIS2_PLACEMENT_3D('',#27295,#16505,#16506);
#13093=AXIS2_PLACEMENT_3D('',#27297,#16508,#16509);
#13094=AXIS2_PLACEMENT_3D('',#27299,#16511,#16512);
#13095=AXIS2_PLACEMENT_3D('',#27300,#16513,#16514);
#13096=AXIS2_PLACEMENT_3D('',#27301,#16515,#16516);
#13097=AXIS2_PLACEMENT_3D('',#27302,#16517,#16518);
#13098=AXIS2_PLACEMENT_3D('',#27303,#16519,#16520);
#13099=AXIS2_PLACEMENT_3D('',#27304,#16521,#16522);
#13100=AXIS2_PLACEMENT_3D('',#27306,#16523,#16524);
#13101=AXIS2_PLACEMENT_3D('',#27309,#16526,#16527);
#13102=AXIS2_PLACEMENT_3D('',#27310,#16528,#16529);
#13103=AXIS2_PLACEMENT_3D('',#27312,#16530,#16531);
#13104=AXIS2_PLACEMENT_3D('',#27315,#16533,#16534);
#13105=AXIS2_PLACEMENT_3D('',#27316,#16535,#16536);
#13106=AXIS2_PLACEMENT_3D('',#27325,#16541,#16542);
#13107=AXIS2_PLACEMENT_3D('',#27331,#16546,#16547);
#13108=AXIS2_PLACEMENT_3D('',#27333,#16548,#16549);
#13109=AXIS2_PLACEMENT_3D('',#27336,#16551,#16552);
#13110=AXIS2_PLACEMENT_3D('',#27337,#16553,#16554);
#13111=AXIS2_PLACEMENT_3D('',#27343,#16558,#16559);
#13112=AXIS2_PLACEMENT_3D('',#27345,#16560,#16561);
#13113=AXIS2_PLACEMENT_3D('',#27348,#16563,#16564);
#13114=AXIS2_PLACEMENT_3D('',#27349,#16565,#16566);
#13115=AXIS2_PLACEMENT_3D('',#27355,#16570,#16571);
#13116=AXIS2_PLACEMENT_3D('',#27357,#16572,#16573);
#13117=AXIS2_PLACEMENT_3D('',#27360,#16575,#16576);
#13118=AXIS2_PLACEMENT_3D('',#27361,#16577,#16578);
#13119=AXIS2_PLACEMENT_3D('',#27367,#16582,#16583);
#13120=AXIS2_PLACEMENT_3D('',#27369,#16584,#16585);
#13121=AXIS2_PLACEMENT_3D('',#27372,#16587,#16588);
#13122=AXIS2_PLACEMENT_3D('',#27373,#16589,#16590);
#13123=AXIS2_PLACEMENT_3D('',#27379,#16594,#16595);
#13124=AXIS2_PLACEMENT_3D('',#27385,#16599,#16600);
#13125=AXIS2_PLACEMENT_3D('',#27388,#16603,#16604);
#13126=AXIS2_PLACEMENT_3D('',#27389,#16605,#16606);
#13127=AXIS2_PLACEMENT_3D('',#27390,#16607,#16608);
#13128=AXIS2_PLACEMENT_3D('',#27392,#16609,#16610);
#13129=AXIS2_PLACEMENT_3D('',#27395,#16612,#16613);
#13130=AXIS2_PLACEMENT_3D('',#27396,#16614,#16615);
#13131=AXIS2_PLACEMENT_3D('',#27398,#16616,#16617);
#13132=AXIS2_PLACEMENT_3D('',#27401,#16619,#16620);
#13133=AXIS2_PLACEMENT_3D('',#27402,#16621,#16622);
#13134=AXIS2_PLACEMENT_3D('',#27411,#16627,#16628);
#13135=AXIS2_PLACEMENT_3D('',#27417,#16632,#16633);
#13136=AXIS2_PLACEMENT_3D('',#27419,#16634,#16635);
#13137=AXIS2_PLACEMENT_3D('',#27422,#16637,#16638);
#13138=AXIS2_PLACEMENT_3D('',#27423,#16639,#16640);
#13139=AXIS2_PLACEMENT_3D('',#27429,#16644,#16645);
#13140=AXIS2_PLACEMENT_3D('',#27431,#16646,#16647);
#13141=AXIS2_PLACEMENT_3D('',#27434,#16649,#16650);
#13142=AXIS2_PLACEMENT_3D('',#27435,#16651,#16652);
#13143=AXIS2_PLACEMENT_3D('',#27441,#16656,#16657);
#13144=AXIS2_PLACEMENT_3D('',#27443,#16658,#16659);
#13145=AXIS2_PLACEMENT_3D('',#27446,#16661,#16662);
#13146=AXIS2_PLACEMENT_3D('',#27447,#16663,#16664);
#13147=AXIS2_PLACEMENT_3D('',#27453,#16668,#16669);
#13148=AXIS2_PLACEMENT_3D('',#27456,#16672,#16673);
#13149=AXIS2_PLACEMENT_3D('',#27457,#16674,#16675);
#13150=AXIS2_PLACEMENT_3D('',#27458,#16676,#16677);
#13151=AXIS2_PLACEMENT_3D('',#27460,#16678,#16679);
#13152=AXIS2_PLACEMENT_3D('',#27463,#16681,#16682);
#13153=AXIS2_PLACEMENT_3D('',#27464,#16683,#16684);
#13154=AXIS2_PLACEMENT_3D('',#27466,#16685,#16686);
#13155=AXIS2_PLACEMENT_3D('',#27469,#16688,#16689);
#13156=AXIS2_PLACEMENT_3D('',#27470,#16690,#16691);
#13157=AXIS2_PLACEMENT_3D('',#27479,#16696,#16697);
#13158=AXIS2_PLACEMENT_3D('',#27485,#16701,#16702);
#13159=AXIS2_PLACEMENT_3D('',#27487,#16703,#16704);
#13160=AXIS2_PLACEMENT_3D('',#27489,#16705,#16706);
#13161=AXIS2_PLACEMENT_3D('',#27491,#16708,#16709);
#13162=AXIS2_PLACEMENT_3D('',#27497,#16713,#16714);
#13163=AXIS2_PLACEMENT_3D('',#27499,#16715,#16716);
#13164=AXIS2_PLACEMENT_3D('',#27501,#16717,#16718);
#13165=AXIS2_PLACEMENT_3D('',#27503,#16720,#16721);
#13166=AXIS2_PLACEMENT_3D('',#27509,#16725,#16726);
#13167=AXIS2_PLACEMENT_3D('',#27511,#16727,#16728);
#13168=AXIS2_PLACEMENT_3D('',#27513,#16729,#16730);
#13169=AXIS2_PLACEMENT_3D('',#27515,#16732,#16733);
#13170=AXIS2_PLACEMENT_3D('',#27521,#16737,#16738);
#13171=AXIS2_PLACEMENT_3D('',#27524,#16741,#16742);
#13172=AXIS2_PLACEMENT_3D('',#27525,#16743,#16744);
#13173=AXIS2_PLACEMENT_3D('',#27526,#16745,#16746);
#13174=AXIS2_PLACEMENT_3D('',#27527,#16747,#16748);
#13175=AXIS2_PLACEMENT_3D('',#27528,#16749,#16750);
#13176=AXIS2_PLACEMENT_3D('',#27529,#16751,#16752);
#13177=DIRECTION('axis',(0.,0.,1.));
#13178=DIRECTION('refdir',(1.,0.,0.));
#13179=DIRECTION('axis',(0.,0.,1.));
#13180=DIRECTION('refdir',(1.,0.,0.));
#13181=DIRECTION('center_axis',(0.,0.,-1.));
#13182=DIRECTION('ref_axis',(-1.,0.,0.));
#13183=DIRECTION('',(0.,0.,-1.));
#13184=DIRECTION('center_axis',(0.,0.,1.));
#13185=DIRECTION('ref_axis',(1.,0.,0.));
#13186=DIRECTION('center_axis',(0.,0.,1.));
#13187=DIRECTION('ref_axis',(1.,0.,0.));
#13188=DIRECTION('center_axis',(0.,0.,1.));
#13189=DIRECTION('ref_axis',(1.,0.,0.));
#13190=DIRECTION('center_axis',(0.,0.,1.));
#13191=DIRECTION('ref_axis',(1.,0.,0.));
#13192=DIRECTION('center_axis',(1.22464679914735E-16,-1.,0.));
#13193=DIRECTION('ref_axis',(-1.,-1.22464679914735E-16,0.));
#13194=DIRECTION('center_axis',(0.,0.,-1.));
#13195=DIRECTION('ref_axis',(1.,0.,0.));
#13196=DIRECTION('center_axis',(0.,0.,-1.));
#13197=DIRECTION('ref_axis',(-1.,0.,0.));
#13198=DIRECTION('center_axis',(0.,0.,-1.));
#13199=DIRECTION('ref_axis',(-1.,0.,0.));
#13200=DIRECTION('',(0.,0.,1.));
#13201=DIRECTION('center_axis',(-5.59912692738561E-15,-5.55111512312578E-15,
-1.));
#13202=DIRECTION('ref_axis',(1.,-2.66519052715287E-31,-5.59912692738561E-15));
#13203=DIRECTION('',(0.,0.,-1.));
#13204=DIRECTION('center_axis',(0.,0.,-1.));
#13205=DIRECTION('ref_axis',(-1.,0.,0.));
#13206=DIRECTION('center_axis',(0.,0.,1.));
#13207=DIRECTION('ref_axis',(-1.,0.,0.));
#13208=DIRECTION('center_axis',(0.,0.,1.));
#13209=DIRECTION('ref_axis',(-1.,0.,0.));
#13210=DIRECTION('',(0.,0.,1.));
#13211=DIRECTION('center_axis',(0.,0.,1.));
#13212=DIRECTION('ref_axis',(1.,0.,0.));
#13213=DIRECTION('',(0.,0.,-1.));
#13214=DIRECTION('center_axis',(0.,0.,-1.));
#13215=DIRECTION('ref_axis',(-1.,0.,0.));
#13216=DIRECTION('center_axis',(0.,0.,-1.));
#13217=DIRECTION('ref_axis',(-1.,0.,0.));
#13218=DIRECTION('',(0.,0.,1.));
#13219=DIRECTION('center_axis',(0.,0.,-1.));
#13220=DIRECTION('ref_axis',(1.,0.,0.));
#13221=DIRECTION('',(0.,0.,-1.));
#13222=DIRECTION('center_axis',(0.,1.,0.));
#13223=DIRECTION('ref_axis',(1.,0.,0.));
#13224=DIRECTION('center_axis',(0.710144927536232,-0.704055524724123,-3.94209624685744E-15));
#13225=DIRECTION('ref_axis',(-0.704055524724123,-0.710144927536232,-5.14874778252965E-31));
#13226=DIRECTION('center_axis',(-1.,-5.55111512312578E-15,0.));
#13227=DIRECTION('ref_axis',(5.55111512312578E-15,-1.,0.));
#13228=DIRECTION('center_axis',(0.,0.,1.));
#13229=DIRECTION('ref_axis',(1.,0.,0.));
#13230=DIRECTION('center_axis',(0.,1.,0.));
#13231=DIRECTION('ref_axis',(1.,0.,0.));
#13232=DIRECTION('center_axis',(0.,0.,-1.));
#13233=DIRECTION('ref_axis',(-1.,0.,0.));
#13234=DIRECTION('center_axis',(-1.,0.,-5.55111512312578E-15));
#13235=DIRECTION('ref_axis',(-5.55111512312578E-15,0.,1.));
#13236=DIRECTION('center_axis',(0.710144927536229,-0.704055524724125,0.));
#13237=DIRECTION('ref_axis',(-0.704055524724125,-0.710144927536229,0.));
#13238=DIRECTION('center_axis',(0.,1.,0.));
#13239=DIRECTION('ref_axis',(1.,0.,0.));
#13240=DIRECTION('center_axis',(-0.710144927536232,0.704055524724123,3.94209624685746E-15));
#13241=DIRECTION('ref_axis',(-0.704055524724123,-0.710144927536232,2.54343028847643E-31));
#13242=DIRECTION('center_axis',(-1.,-5.55111512312578E-15,0.));
#13243=DIRECTION('ref_axis',(5.55111512312578E-15,-1.,0.));
#13244=DIRECTION('center_axis',(-7.88448485693075E-15,0.,-1.));
#13245=DIRECTION('ref_axis',(1.,0.,-7.88448485693075E-15));
#13246=DIRECTION('center_axis',(0.,1.,0.));
#13247=DIRECTION('ref_axis',(1.,0.,0.));
#13248=DIRECTION('center_axis',(0.,0.,1.));
#13249=DIRECTION('ref_axis',(-1.,0.,0.));
#13250=DIRECTION('center_axis',(-1.,0.,-5.55111512312578E-15));
#13251=DIRECTION('ref_axis',(-5.55111512312578E-15,0.,1.));
#13252=DIRECTION('center_axis',(-0.710144927536229,0.704055524724125,0.));
#13253=DIRECTION('ref_axis',(-0.704055524724125,-0.710144927536229,0.));
#13254=DIRECTION('center_axis',(0.,0.,1.));
#13255=DIRECTION('ref_axis',(1.,0.,0.));
#13256=DIRECTION('center_axis',(0.,0.,1.));
#13257=DIRECTION('ref_axis',(1.,0.,0.));
#13258=DIRECTION('center_axis',(1.22464679914735E-16,-1.,0.));
#13259=DIRECTION('ref_axis',(-1.,-1.22464679914735E-16,0.));
#13260=DIRECTION('center_axis',(0.,0.,-1.));
#13261=DIRECTION('ref_axis',(1.,0.,0.));
#13262=DIRECTION('center_axis',(0.,0.,-1.));
#13263=DIRECTION('ref_axis',(1.,0.,0.));
#13264=DIRECTION('center_axis',(0.,0.,1.));
#13265=DIRECTION('ref_axis',(1.,0.,0.));
#13266=DIRECTION('center_axis',(0.,0.,1.));
#13267=DIRECTION('ref_axis',(1.,0.,0.));
#13268=DIRECTION('center_axis',(0.,0.,1.));
#13269=DIRECTION('ref_axis',(1.,0.,0.));
#13270=DIRECTION('center_axis',(1.22464679914735E-16,-1.,0.));
#13271=DIRECTION('ref_axis',(-1.,-1.22464679914735E-16,0.));
#13272=DIRECTION('center_axis',(0.,0.,-1.));
#13273=DIRECTION('ref_axis',(1.,0.,0.));
#13274=DIRECTION('center_axis',(0.,0.,1.));
#13275=DIRECTION('ref_axis',(1.,0.,0.));
#13276=DIRECTION('center_axis',(0.,0.,1.));
#13277=DIRECTION('ref_axis',(1.,0.,0.));
#13278=DIRECTION('',(-0.707106781186566,-8.65956056235516E-17,0.707106781186529));
#13279=DIRECTION('center_axis',(0.,0.,1.));
#13280=DIRECTION('ref_axis',(1.,0.,0.));
#13281=DIRECTION('center_axis',(0.,0.,1.));
#13282=DIRECTION('ref_axis',(1.,0.,0.));
#13283=DIRECTION('center_axis',(0.,0.,1.));
#13284=DIRECTION('ref_axis',(1.,0.,0.));
#13285=DIRECTION('',(0.,0.,1.));
#13286=DIRECTION('center_axis',(0.,0.,1.));
#13287=DIRECTION('ref_axis',(1.,0.,0.));
#13288=DIRECTION('center_axis',(0.,0.,1.));
#13289=DIRECTION('ref_axis',(1.,0.,0.));
#13290=DIRECTION('',(-0.707106781186566,-8.65956056235516E-17,0.707106781186529));
#13291=DIRECTION('center_axis',(0.,0.,1.));
#13292=DIRECTION('ref_axis',(1.,0.,0.));
#13293=DIRECTION('center_axis',(0.,0.,1.));
#13294=DIRECTION('ref_axis',(1.,0.,0.));
#13295=DIRECTION('center_axis',(0.,0.,1.));
#13296=DIRECTION('ref_axis',(1.,0.,0.));
#13297=DIRECTION('',(0.,0.,1.));
#13298=DIRECTION('center_axis',(0.,0.,1.));
#13299=DIRECTION('ref_axis',(1.,0.,0.));
#13300=DIRECTION('center_axis',(0.,0.,1.));
#13301=DIRECTION('ref_axis',(1.,0.,0.));
#13302=DIRECTION('',(-0.707106781186558,-8.65956056235506E-17,0.707106781186537));
#13303=DIRECTION('center_axis',(0.,0.,1.));
#13304=DIRECTION('ref_axis',(1.,0.,0.));
#13305=DIRECTION('center_axis',(0.,0.,1.));
#13306=DIRECTION('ref_axis',(1.,0.,0.));
#13307=DIRECTION('center_axis',(0.,0.,1.));
#13308=DIRECTION('ref_axis',(1.,0.,0.));
#13309=DIRECTION('',(0.,0.,1.));
#13310=DIRECTION('center_axis',(0.,0.,1.));
#13311=DIRECTION('ref_axis',(1.,0.,0.));
#13312=DIRECTION('center_axis',(0.,0.,1.));
#13313=DIRECTION('ref_axis',(1.,0.,0.));
#13314=DIRECTION('',(-0.707106781186566,-8.65956056235516E-17,0.707106781186529));
#13315=DIRECTION('center_axis',(0.,0.,1.));
#13316=DIRECTION('ref_axis',(1.,0.,0.));
#13317=DIRECTION('center_axis',(0.,0.,1.));
#13318=DIRECTION('ref_axis',(1.,0.,0.));
#13319=DIRECTION('center_axis',(0.,0.,1.));
#13320=DIRECTION('ref_axis',(1.,0.,0.));
#13321=DIRECTION('',(0.,0.,1.));
#13322=DIRECTION('center_axis',(0.,0.,1.));
#13323=DIRECTION('ref_axis',(1.,0.,0.));
#13324=DIRECTION('center_axis',(0.,0.,1.));
#13325=DIRECTION('ref_axis',(1.,0.,0.));
#13326=DIRECTION('',(-0.707106781186566,-8.65956056235516E-17,0.707106781186529));
#13327=DIRECTION('center_axis',(0.,0.,1.));
#13328=DIRECTION('ref_axis',(1.,0.,0.));
#13329=DIRECTION('center_axis',(0.,0.,1.));
#13330=DIRECTION('ref_axis',(1.,0.,0.));
#13331=DIRECTION('center_axis',(0.,0.,1.));
#13332=DIRECTION('ref_axis',(1.,0.,0.));
#13333=DIRECTION('',(0.,0.,1.));
#13334=DIRECTION('center_axis',(0.,0.,1.));
#13335=DIRECTION('ref_axis',(1.,0.,0.));
#13336=DIRECTION('center_axis',(0.,0.,1.));
#13337=DIRECTION('ref_axis',(1.,0.,0.));
#13338=DIRECTION('',(-0.707106781186558,-8.65956056235506E-17,0.707106781186537));
#13339=DIRECTION('center_axis',(0.,0.,1.));
#13340=DIRECTION('ref_axis',(1.,0.,0.));
#13341=DIRECTION('center_axis',(0.,0.,1.));
#13342=DIRECTION('ref_axis',(1.,0.,0.));
#13343=DIRECTION('center_axis',(0.,0.,1.));
#13344=DIRECTION('ref_axis',(1.,0.,0.));
#13345=DIRECTION('',(0.,0.,1.));
#13346=DIRECTION('center_axis',(0.,0.,-1.));
#13347=DIRECTION('ref_axis',(-1.,0.,0.));
#13348=DIRECTION('',(0.,0.,1.));
#13349=DIRECTION('center_axis',(0.,0.,-1.));
#13350=DIRECTION('ref_axis',(-1.,0.,0.));
#13351=DIRECTION('center_axis',(0.,0.,-1.));
#13352=DIRECTION('ref_axis',(1.,0.,0.));
#13353=DIRECTION('',(0.707106781186562,-8.65956056235511E-17,-0.707106781186533));
#13354=DIRECTION('center_axis',(0.,0.,1.));
#13355=DIRECTION('ref_axis',(1.,0.,0.));
#13356=DIRECTION('center_axis',(0.,0.,1.));
#13357=DIRECTION('ref_axis',(1.,0.,0.));
#13358=DIRECTION('center_axis',(0.,0.,1.));
#13359=DIRECTION('ref_axis',(1.,0.,0.));
#13360=DIRECTION('center_axis',(0.,0.,1.));
#13361=DIRECTION('ref_axis',(1.,0.,0.));
#13362=DIRECTION('',(-0.707106781186562,-8.65956056235511E-17,0.707106781186533));
#13363=DIRECTION('center_axis',(0.,0.,-1.));
#13364=DIRECTION('ref_axis',(1.,0.,0.));
#13365=DIRECTION('center_axis',(0.,0.,-1.));
#13366=DIRECTION('ref_axis',(-1.,0.,0.));
#13367=DIRECTION('',(0.,0.,-1.));
#13368=DIRECTION('center_axis',(0.,-1.,0.));
#13369=DIRECTION('ref_axis',(0.,0.,-1.));
#13370=DIRECTION('center_axis',(0.,-1.,0.));
#13371=DIRECTION('ref_axis',(0.,0.,-1.));
#13372=DIRECTION('',(0.,-1.,0.));
#13373=DIRECTION('center_axis',(0.,-1.,0.));
#13374=DIRECTION('ref_axis',(0.,0.,-1.));
#13375=DIRECTION('center_axis',(0.,-1.,0.));
#13376=DIRECTION('ref_axis',(0.,0.,-1.));
#13377=DIRECTION('center_axis',(0.,-1.,0.));
#13378=DIRECTION('ref_axis',(0.,0.,-1.));
#13379=DIRECTION('',(0.,-1.,0.));
#13380=DIRECTION('center_axis',(0.,-1.,0.));
#13381=DIRECTION('ref_axis',(0.,0.,-1.));
#13382=DIRECTION('center_axis',(0.,-1.,0.));
#13383=DIRECTION('ref_axis',(0.,0.,-1.));
#13384=DIRECTION('center_axis',(0.,1.,0.));
#13385=DIRECTION('ref_axis',(0.,0.,1.));
#13386=DIRECTION('',(0.,-1.,0.));
#13387=DIRECTION('center_axis',(0.,-1.,0.));
#13388=DIRECTION('ref_axis',(0.,0.,-1.));
#13389=DIRECTION('center_axis',(0.,-1.,0.));
#13390=DIRECTION('ref_axis',(0.,0.,-1.));
#13391=DIRECTION('center_axis',(0.,1.,0.));
#13392=DIRECTION('ref_axis',(0.,0.,1.));
#13393=DIRECTION('',(0.,-1.,0.));
#13394=DIRECTION('center_axis',(0.,-1.,0.));
#13395=DIRECTION('ref_axis',(0.,0.,-1.));
#13396=DIRECTION('center_axis',(2.52323414687536E-16,0.,1.));
#13397=DIRECTION('ref_axis',(1.,0.,-2.52323414687536E-16));
#13398=DIRECTION('center_axis',(-8.7764665978268E-18,-5.25222157317359E-18,
1.));
#13399=DIRECTION('ref_axis',(1.,-4.60959472013434E-35,8.7764665978268E-18));
#13400=DIRECTION('',(2.52323414687536E-16,0.,1.));
#13401=DIRECTION('center_axis',(2.52323414687536E-16,0.,1.));
#13402=DIRECTION('ref_axis',(1.,0.,-2.52323414687536E-16));
#13403=DIRECTION('',(0.,0.,-1.));
#13404=DIRECTION('center_axis',(0.,0.,-1.));
#13405=DIRECTION('ref_axis',(-1.,0.,0.));
#13406=DIRECTION('center_axis',(0.,0.,1.));
#13407=DIRECTION('ref_axis',(1.,0.,0.));
#13408=DIRECTION('center_axis',(0.,0.,1.));
#13409=DIRECTION('ref_axis',(-1.,-4.44089209850063E-15,0.));
#13410=DIRECTION('',(0.,0.,-1.));
#13411=DIRECTION('center_axis',(0.,0.,1.));
#13412=DIRECTION('ref_axis',(1.,0.,0.));
#13413=DIRECTION('',(-2.52323414687536E-16,0.,-1.));
#13414=DIRECTION('center_axis',(2.52323414687536E-16,0.,1.));
#13415=DIRECTION('ref_axis',(1.,0.,-2.52323414687536E-16));
#13416=DIRECTION('center_axis',(0.,0.,1.));
#13417=DIRECTION('ref_axis',(1.,0.,0.));
#13418=DIRECTION('center_axis',(0.,0.,1.));
#13419=DIRECTION('ref_axis',(1.,0.,0.));
#13420=DIRECTION('',(0.,0.,-1.));
#13421=DIRECTION('center_axis',(0.,0.,1.));
#13422=DIRECTION('ref_axis',(1.,0.,0.));
#13423=DIRECTION('center_axis',(0.,0.,1.));
#13424=DIRECTION('ref_axis',(1.,0.,0.));
#13425=DIRECTION('',(2.52323414687536E-16,0.,1.));
#13426=DIRECTION('center_axis',(0.,0.,-1.));
#13427=DIRECTION('ref_axis',(-1.,0.,0.));
#13428=DIRECTION('',(0.,0.,1.));
#13429=DIRECTION('',(0.,0.,-1.));
#13430=DIRECTION('',(0.,0.,1.));
#13431=DIRECTION('center_axis',(0.,0.,1.));
#13432=DIRECTION('ref_axis',(1.,0.,0.));
#13433=DIRECTION('center_axis',(2.52323414687536E-16,0.,1.));
#13434=DIRECTION('ref_axis',(-1.,-4.44089209850063E-15,2.52323414687536E-16));
#13435=DIRECTION('center_axis',(-2.52323414687536E-16,0.,-1.));
#13436=DIRECTION('ref_axis',(1.,-4.44089209850063E-15,-2.52323414687536E-16));
#13437=DIRECTION('center_axis',(0.,0.,1.));
#13438=DIRECTION('ref_axis',(1.,0.,0.));
#13439=DIRECTION('',(0.,0.,-1.));
#13440=DIRECTION('center_axis',(0.,0.,-1.));
#13441=DIRECTION('ref_axis',(1.,0.,0.));
#13442=DIRECTION('center_axis',(0.,0.,-1.));
#13443=DIRECTION('ref_axis',(1.,0.,0.));
#13444=DIRECTION('',(0.,0.,1.));
#13445=DIRECTION('center_axis',(0.,0.,1.));
#13446=DIRECTION('ref_axis',(1.,0.,0.));
#13447=DIRECTION('center_axis',(0.,0.,1.));
#13448=DIRECTION('ref_axis',(-1.,0.,0.));
#13449=DIRECTION('',(0.,0.,-1.));
#13450=DIRECTION('center_axis',(0.,0.,-1.));
#13451=DIRECTION('ref_axis',(-1.,0.,0.));
#13452=DIRECTION('center_axis',(0.,0.,-1.));
#13453=DIRECTION('ref_axis',(1.,0.,0.));
#13454=DIRECTION('',(0.,0.,1.));
#13455=DIRECTION('center_axis',(0.,0.,1.));
#13456=DIRECTION('ref_axis',(1.,0.,0.));
#13457=DIRECTION('',(0.,0.,1.));
#13458=DIRECTION('center_axis',(0.,0.,-1.));
#13459=DIRECTION('ref_axis',(-1.,0.,0.));
#13460=DIRECTION('',(0.,0.,1.));
#13461=DIRECTION('center_axis',(0.,0.,1.));
#13462=DIRECTION('ref_axis',(-1.,0.,0.));
#13463=DIRECTION('',(0.,0.,1.));
#13464=DIRECTION('center_axis',(0.,0.,1.));
#13465=DIRECTION('ref_axis',(1.,0.,0.));
#13466=DIRECTION('',(0.,0.,-1.));
#13467=DIRECTION('center_axis',(0.,0.,-1.));
#13468=DIRECTION('ref_axis',(1.,1.06581410364015E-14,0.));
#13469=DIRECTION('',(0.,0.,1.));
#13470=DIRECTION('center_axis',(0.,1.,0.));
#13471=DIRECTION('ref_axis',(0.,0.,1.));
#13472=DIRECTION('',(1.,0.,0.));
#13473=DIRECTION('',(0.,0.,1.));
#13474=DIRECTION('',(-1.,0.,0.));
#13475=DIRECTION('',(-0.707106781186547,0.,-0.707106781186547));
#13476=DIRECTION('',(0.,0.,-1.));
#13477=DIRECTION('',(0.707106781186547,0.,-0.707106781186547));
#13478=DIRECTION('center_axis',(0.,-1.,0.));
#13479=DIRECTION('ref_axis',(0.,0.,-1.));
#13480=DIRECTION('',(-0.707106781186547,0.,0.707106781186547));
#13481=DIRECTION('',(0.,0.,1.));
#13482=DIRECTION('',(0.707106781186547,0.,0.707106781186547));
#13483=DIRECTION('',(1.,0.,0.));
#13484=DIRECTION('',(0.,0.,-1.));
#13485=DIRECTION('',(-1.,0.,0.));
#13486=DIRECTION('center_axis',(0.,1.,0.));
#13487=DIRECTION('ref_axis',(0.,0.,-1.));
#13488=DIRECTION('',(0.,0.,-1.));
#13489=DIRECTION('center_axis',(0.,1.,0.));
#13490=DIRECTION('ref_axis',(0.,0.,-1.));
#13491=DIRECTION('',(1.,0.,0.));
#13492=DIRECTION('',(0.,0.,-1.));
#13493=DIRECTION('',(-1.,0.,0.));
#13494=DIRECTION('center_axis',(0.,1.,0.));
#13495=DIRECTION('ref_axis',(0.,0.,-1.));
#13496=DIRECTION('',(0.,0.,-1.));
#13497=DIRECTION('center_axis',(0.,1.,0.));
#13498=DIRECTION('ref_axis',(0.,0.,-1.));
#13499=DIRECTION('',(1.,0.,0.));
#13500=DIRECTION('',(0.,0.,-1.));
#13501=DIRECTION('',(-1.,0.,0.));
#13502=DIRECTION('center_axis',(0.,1.,0.));
#13503=DIRECTION('ref_axis',(0.,0.,1.));
#13504=DIRECTION('',(-1.,0.,0.));
#13505=DIRECTION('',(1.,0.,0.));
#13506=DIRECTION('',(0.707106781186548,0.,-0.707106781186548));
#13507=DIRECTION('',(0.,0.,-1.));
#13508=DIRECTION('',(-0.707106781186547,0.,-0.707106781186547));
#13509=DIRECTION('',(-1.,0.,0.));
#13510=DIRECTION('',(1.,0.,0.));
#13511=DIRECTION('center_axis',(0.,1.,0.));
#13512=DIRECTION('ref_axis',(0.,0.,1.));
#13513=DIRECTION('',(0.,0.,1.));
#13514=DIRECTION('center_axis',(0.,1.,0.));
#13515=DIRECTION('ref_axis',(0.,0.,1.));
#13516=DIRECTION('',(-1.,0.,0.));
#13517=DIRECTION('',(1.,0.,0.));
#13518=DIRECTION('center_axis',(0.,1.,0.));
#13519=DIRECTION('ref_axis',(0.,0.,1.));
#13520=DIRECTION('',(0.,0.,1.));
#13521=DIRECTION('center_axis',(0.,1.,0.));
#13522=DIRECTION('ref_axis',(0.,0.,1.));
#13523=DIRECTION('center_axis',(0.,0.,1.));
#13524=DIRECTION('ref_axis',(1.,0.,0.));
#13525=DIRECTION('center_axis',(-2.52323414687536E-16,0.,-1.));
#13526=DIRECTION('ref_axis',(-1.,0.,2.52323414687536E-16));
#13527=DIRECTION('center_axis',(-2.52323414687536E-16,0.,-1.));
#13528=DIRECTION('ref_axis',(1.,5.15143483426073E-14,-2.52323414687536E-16));
#13529=DIRECTION('center_axis',(2.52323414687536E-16,0.,1.));
#13530=DIRECTION('ref_axis',(-1.,4.9737991503207E-14,2.52323414687536E-16));
#13531=DIRECTION('',(-2.52323414687536E-16,0.,-1.));
#13532=DIRECTION('center_axis',(-2.52323414687536E-16,0.,-1.));
#13533=DIRECTION('ref_axis',(-1.,0.,2.52323414687536E-16));
#13534=DIRECTION('center_axis',(-2.52323414687536E-16,0.,-1.));
#13535=DIRECTION('ref_axis',(-1.,0.,2.52323414687536E-16));
#13536=DIRECTION('center_axis',(-2.52323414687536E-16,0.,-1.));
#13537=DIRECTION('ref_axis',(-1.,0.,2.52323414687536E-16));
#13538=DIRECTION('center_axis',(2.52323414687536E-16,0.,1.));
#13539=DIRECTION('ref_axis',(-1.,1.77635683940025E-15,2.52323414687536E-16));
#13540=DIRECTION('',(3.46944695195362E-15,-1.,-8.754227019942E-31));
#13541=DIRECTION('center_axis',(-2.52323414687536E-16,0.,-1.));
#13542=DIRECTION('ref_axis',(-1.,0.,2.52323414687536E-16));
#13543=DIRECTION('center_axis',(-2.52323414687536E-16,0.,-1.));
#13544=DIRECTION('ref_axis',(-1.,0.,2.52323414687536E-16));
#13545=DIRECTION('center_axis',(2.52323414687536E-16,0.,1.));
#13546=DIRECTION('ref_axis',(1.,0.,-2.52323414687536E-16));
#13547=DIRECTION('center_axis',(-0.0237269141195627,-0.851557493622926,
0.523724038593803));
#13548=DIRECTION('ref_axis',(-0.0385579135341051,0.524261227788714,0.85068410843354));
#13549=DIRECTION('',(-3.04630100940178E-45,8.57457505675013E-31,-1.));
#13550=DIRECTION('center_axis',(-0.0237269141195507,-0.851557493623381,
-0.523724038593063));
#13551=DIRECTION('ref_axis',(0.0146007549783791,0.523520473997797,-0.851887980464089));
#13552=DIRECTION('center_axis',(-2.52323414687536E-16,0.,-1.));
#13553=DIRECTION('ref_axis',(-1.,0.,2.52323414687536E-16));
#13554=DIRECTION('center_axis',(2.52323414687536E-16,0.,1.));
#13555=DIRECTION('ref_axis',(1.,0.,-2.52323414687536E-16));
#13556=DIRECTION('center_axis',(-2.52323414687536E-16,0.,-1.));
#13557=DIRECTION('ref_axis',(1.,-8.88178419700125E-16,-2.52323414687536E-16));
#13558=DIRECTION('center_axis',(2.52323414687536E-16,0.,1.));
#13559=DIRECTION('ref_axis',(1.,0.,-2.52323414687536E-16));
#13560=DIRECTION('center_axis',(2.52323414687536E-16,0.,1.));
#13561=DIRECTION('ref_axis',(1.,0.,-2.52323414687536E-16));
#13562=DIRECTION('center_axis',(2.52323414687536E-16,0.,1.));
#13563=DIRECTION('ref_axis',(1.,0.,-2.52323414687536E-16));
#13564=DIRECTION('',(-3.46944695195361E-15,1.,8.75422701994197E-31));
#13565=DIRECTION('center_axis',(-1.,-3.46944695195361E-15,2.41352831440251E-16));
#13566=DIRECTION('ref_axis',(3.46944695195361E-15,-1.,-4.87884146037003E-48));
#13567=DIRECTION('',(3.46944695195361E-15,-1.,0.));
#13568=DIRECTION('center_axis',(-1.,-5.52038264252701E-15,6.2479767589266E-16));
#13569=DIRECTION('ref_axis',(-4.16417573426786E-15,0.819231920519141,0.573462344363185));
#13570=DIRECTION('',(2.41352831440251E-16,0.,1.));
#13571=DIRECTION('center_axis',(-1.,-1.42770121134483E-15,3.50862385444968E-15));
#13572=DIRECTION('ref_axis',(-3.18168206635957E-15,0.819231920518936,-0.573462344363477));
#13573=DIRECTION('',(-3.46944695195361E-15,1.,0.));
#13574=DIRECTION('center_axis',(-1.,-8.96139251667977E-15,-8.32782443095335E-16));
#13575=DIRECTION('ref_axis',(8.32782443102262E-16,-7.72993066836482E-13,
-1.));
#13576=DIRECTION('',(-2.41352831440251E-16,0.,-1.));
#13577=DIRECTION('center_axis',(-1.,0.,0.));
#13578=DIRECTION('ref_axis',(0.,-5.23876817808574E-13,-1.));
#13579=DIRECTION('',(3.46944695195361E-15,-1.,1.91404262256119E-33));
#13580=DIRECTION('center_axis',(-1.,-1.17134969274264E-14,8.78564447069424E-15));
#13581=DIRECTION('ref_axis',(-8.78564447074124E-15,4.012053825336E-12,-1.));
#13582=DIRECTION('',(-2.41352831440251E-16,0.,-1.));
#13583=DIRECTION('center_axis',(-1.,-4.85188929015585E-15,-1.99030797820559E-15));
#13584=DIRECTION('ref_axis',(1.99030797821407E-15,-1.7484297207494E-12,
-1.));
#13585=DIRECTION('',(-3.46944695195361E-15,1.,0.));
#13586=DIRECTION('center_axis',(-1.,-6.86244039359303E-15,6.93075172121948E-15));
#13587=DIRECTION('ref_axis',(-9.59645535334076E-15,0.819231920519237,-0.573462344363048));
#13588=DIRECTION('',(2.41352831440251E-16,-1.24480026177148E-32,1.));
#13589=DIRECTION('center_axis',(-1.,6.86244039359302E-15,6.93075172121946E-15));
#13590=DIRECTION('ref_axis',(9.5964553533418E-15,0.819231920518884,0.573462344363551));
#13591=DIRECTION('center_axis',(3.5527136788005E-15,-1.,-8.57457505675013E-31));
#13592=DIRECTION('ref_axis',(1.,3.5527136788005E-15,0.));
#13593=DIRECTION('center_axis',(3.5527136788005E-15,-1.,-8.57457505675013E-31));
#13594=DIRECTION('ref_axis',(1.,3.5527136788005E-15,-1.26929208725074E-46));
#13595=DIRECTION('',(-0.99034174667433,-3.51840067009707E-15,-0.138647844534406));
#13596=DIRECTION('',(0.99034174667433,3.51840067009707E-15,-0.138647844534406));
#13597=DIRECTION('center_axis',(3.5527136788005E-15,-1.,-8.57457505675013E-31));
#13598=DIRECTION('ref_axis',(1.,3.5527136788005E-15,-1.26929208725074E-46));
#13599=DIRECTION('center_axis',(-0.138647844534406,-4.81031341614835E-16,
-0.99034174667433));
#13600=DIRECTION('ref_axis',(-0.99034174667433,3.0510584428262E-33,0.138647844534406));
#13601=DIRECTION('',(0.9714691757235,0.194293835144703,-0.13600568460129));
#13602=DIRECTION('center_axis',(-0.138647844534404,-4.3608853103437E-15,
-0.990341746674331));
#13603=DIRECTION('ref_axis',(-0.142395756615647,0.989609027893549,0.0199354059261866));
#13604=DIRECTION('',(-3.46944695195362E-15,1.,8.93770063475844E-31));
#13605=DIRECTION('',(-0.99034174667433,-3.51840067009707E-15,0.138647844534406));
#13606=DIRECTION('center_axis',(-0.138647844534406,-4.81031341614834E-16,
0.99034174667433));
#13607=DIRECTION('ref_axis',(0.99034174667433,1.28749462997746E-32,0.138647844534406));
#13608=DIRECTION('',(3.46944695195361E-15,-1.,-8.93770063475844E-31));
#13609=DIRECTION('center_axis',(-0.138647844534388,-1.15563460846761E-13,
0.990341746674333));
#13610=DIRECTION('ref_axis',(-0.192413756189552,0.980944083309055,-0.0269379258664217));
#13611=DIRECTION('',(-0.9714691757235,-0.194293835144703,-0.13600568460129));
#13612=DIRECTION('',(0.99034174667433,3.51840067009707E-15,0.138647844534406));
#13613=DIRECTION('center_axis',(-0.196116135138187,0.98058067569092,4.73331845067205E-17));
#13614=DIRECTION('ref_axis',(-0.980580675690919,-0.196116135138187,9.12179048335121E-36));
#13615=DIRECTION('',(0.9714691757235,0.194293835144703,0.13600568460129));
#13616=DIRECTION('',(2.51901469178025E-16,2.10972754755468E-18,1.));
#13617=DIRECTION('',(-0.9714691757235,-0.194293835144703,0.13600568460129));
#13618=DIRECTION('center_axis',(3.46944695195362E-15,-1.,-8.754227019942E-31));
#13619=DIRECTION('ref_axis',(1.,3.46944695195362E-15,0.));
#13620=DIRECTION('center_axis',(0.0303922984798993,0.807916267226531,0.588513052823688));
#13621=DIRECTION('ref_axis',(-0.0416915731841444,0.589297297589034,-0.806839827834306));
#13622=DIRECTION('center_axis',(-3.5527136788005E-15,1.,8.57457505675013E-31));
#13623=DIRECTION('ref_axis',(1.,3.5527136788005E-15,1.90393813087611E-46));
#13624=DIRECTION('center_axis',(-2.52323414687536E-16,0.,-1.));
#13625=DIRECTION('ref_axis',(-1.,0.,2.52323414687536E-16));
#13626=DIRECTION('center_axis',(-2.52323414687536E-16,0.,-1.));
#13627=DIRECTION('ref_axis',(1.,0.,-2.52323414687536E-16));
#13628=DIRECTION('center_axis',(2.52323414687536E-16,0.,1.));
#13629=DIRECTION('ref_axis',(-1.,-1.85962356624714E-14,2.52323414687536E-16));
#13630=DIRECTION('center_axis',(0.185712190755878,-2.42469285118642E-13,
0.982604183893317));
#13631=DIRECTION('ref_axis',(-0.189474179318918,0.981232457104028,0.0358106198915277));
#13632=DIRECTION('center_axis',(0.185712190755882,-2.44440580120635E-13,
-0.982604183893317));
#13633=DIRECTION('ref_axis',(-0.140198967511934,0.98976872371543,-0.0264976048600095));
#13634=DIRECTION('center_axis',(-3.46944695195361E-15,1.,8.75422701994197E-31));
#13635=DIRECTION('ref_axis',(-1.,-3.46944695195361E-15,6.22301527786114E-61));
#13636=DIRECTION('center_axis',(-3.5527136788005E-15,1.,8.57457505675013E-31));
#13637=DIRECTION('ref_axis',(1.,3.5527136788005E-15,1.90393813087611E-46));
#13638=DIRECTION('center_axis',(0.0303922984798813,0.807916267226852,-0.588513052823249));
#13639=DIRECTION('ref_axis',(0.0221372134653148,0.588096554362881,0.808487715754852));
#13640=DIRECTION('center_axis',(-0.9714691757235,-0.194293835144704,-0.13600568460129));
#13641=DIRECTION('ref_axis',(0.196116135138187,-0.98058067569092,-3.92731709847666E-18));
#13642=DIRECTION('center_axis',(0.9714691757235,0.194293835144703,0.136005684601291));
#13643=DIRECTION('ref_axis',(-0.196116135138187,0.98058067569092,3.24008523737298E-18));
#13644=DIRECTION('center_axis',(0.980051041638971,0.143785099769423,0.137207145829456));
#13645=DIRECTION('ref_axis',(-0.145157949036735,0.989408494925856,2.07268495050659E-17));
#13646=DIRECTION('center_axis',(0.999978809045156,0.00651010450232906,-3.96499820692563E-16));
#13647=DIRECTION('ref_axis',(-0.00651010450232906,0.999978809045156,6.00796001774974E-35));
#13648=DIRECTION('center_axis',(2.52323414687536E-16,0.,1.));
#13649=DIRECTION('ref_axis',(1.,0.,-2.507797890918E-16));
#13650=DIRECTION('center_axis',(0.994514519537326,-0.104598615810349,-3.94333184969416E-16));
#13651=DIRECTION('ref_axis',(0.104598615810349,0.994514519537326,5.49398292351409E-33));
#13652=DIRECTION('center_axis',(2.52323414687536E-16,0.,1.));
#13653=DIRECTION('ref_axis',(1.,0.,-2.3201395453391E-16));
#13654=DIRECTION('center_axis',(-0.9714691757235,-0.194293835144704,0.13600568460129));
#13655=DIRECTION('ref_axis',(0.196116135138187,-0.98058067569092,7.05725267053878E-18));
#13656=DIRECTION('center_axis',(0.9714691757235,0.194293835144703,-0.13600568460129));
#13657=DIRECTION('ref_axis',(-0.196116135138187,0.98058067569092,-4.37148606784657E-18));
#13658=DIRECTION('center_axis',(0.980051041638971,0.143785099769423,-0.137207145829457));
#13659=DIRECTION('ref_axis',(-0.145157949036735,0.989408494925857,5.49111790108275E-17));
#13660=DIRECTION('center_axis',(0.999978809045156,0.00651010450232827,-3.96499820692563E-16));
#13661=DIRECTION('ref_axis',(-0.00651010450232827,0.999978809045156,2.30522657691445E-35));
#13662=DIRECTION('center_axis',(-2.52323414687536E-16,0.,-1.));
#13663=DIRECTION('ref_axis',(-1.,0.,2.507797890918E-16));
#13664=DIRECTION('center_axis',(0.994514519537326,-0.104598615810349,-3.94333184969416E-16));
#13665=DIRECTION('ref_axis',(0.104598615810349,0.994514519537326,5.49398292351409E-33));
#13666=DIRECTION('center_axis',(-2.52323414687536E-16,0.,-1.));
#13667=DIRECTION('ref_axis',(-1.,0.,2.3201395453391E-16));
#13668=DIRECTION('center_axis',(-0.99034174667433,-3.51840067009707E-15,
-0.138647844534406));
#13669=DIRECTION('ref_axis',(-0.138647844534406,-3.36051524361832E-32,0.99034174667433));
#13670=DIRECTION('center_axis',(0.99034174667433,3.14142916972953E-15,0.138647844534406));
#13671=DIRECTION('ref_axis',(0.138647844534406,-8.69074855760808E-32,-0.99034174667433));
#13672=DIRECTION('center_axis',(3.5527136788005E-15,-1.,-8.57457505675013E-31));
#13673=DIRECTION('ref_axis',(1.,3.5109170472852E-15,0.));
#13674=DIRECTION('center_axis',(0.998667820387802,2.79231993889397E-15,
0.0516002376145364));
#13675=DIRECTION('ref_axis',(0.0516002376145364,-2.37256198805332E-32,-0.998667820387802));
#13676=DIRECTION('center_axis',(0.999611719795952,-0.0278641283118466,-3.96354266786649E-16));
#13677=DIRECTION('ref_axis',(0.0278641283118466,0.999611719795952,-1.9098216440265E-32));
#13678=DIRECTION('center_axis',(2.52323414687536E-16,0.,1.));
#13679=DIRECTION('ref_axis',(1.,0.,-2.49313240617579E-16));
#13680=DIRECTION('center_axis',(-0.99034174667433,-3.51840067009707E-15,
0.138647844534406));
#13681=DIRECTION('ref_axis',(0.138647844534406,-3.67558502487976E-34,0.99034174667433));
#13682=DIRECTION('center_axis',(0.99034174667433,3.14142916972953E-15,-0.138647844534406));
#13683=DIRECTION('ref_axis',(-0.138647844534406,-1.13235899567505E-30,-0.99034174667433));
#13684=DIRECTION('center_axis',(3.5527136788005E-15,-1.,-8.57457505675013E-31));
#13685=DIRECTION('ref_axis',(1.,3.5109170472852E-15,0.));
#13686=DIRECTION('center_axis',(0.998667820387802,3.56382002618601E-15,
-0.0516002376145376));
#13687=DIRECTION('ref_axis',(-0.0516002376145376,-4.64884186281675E-32,
-0.998667820387802));
#13688=DIRECTION('center_axis',(0.999611719795952,-0.0278641283118465,-3.74257554777419E-16));
#13689=DIRECTION('ref_axis',(0.0278641283118465,0.999611719795952,-1.41173314945589E-33));
#13690=DIRECTION('center_axis',(-2.52323414687536E-16,0.,-1.));
#13691=DIRECTION('ref_axis',(-1.,0.,2.49313240617579E-16));
#13692=DIRECTION('center_axis',(0.935358342755929,-0.353701527614572,-8.65380307002384E-16));
#13693=DIRECTION('ref_axis',(0.353701527614572,0.935358342755929,3.79648143258003E-33));
#13694=DIRECTION('center_axis',(-2.52323414687536E-16,0.,-1.));
#13695=DIRECTION('ref_axis',(-1.,0.,2.1316282072803E-16));
#13696=DIRECTION('center_axis',(0.996895904609183,0.0787309048178608,-4.61156994354849E-16));
#13697=DIRECTION('ref_axis',(-0.0787309048178608,0.996895904609183,8.19223082641905E-33));
#13698=DIRECTION('center_axis',(-0.996895904609183,-0.0787309048178614,
1.15289248588712E-16));
#13699=DIRECTION('ref_axis',(0.0787309048178614,-0.996895904609183,1.91107223648995E-33));
#13700=DIRECTION('center_axis',(2.52323414687536E-16,0.,1.));
#13701=DIRECTION('ref_axis',(1.,0.,-2.1316282072803E-16));
#13702=DIRECTION('center_axis',(-0.93535834275593,0.353701527614571,8.65380307002384E-16));
#13703=DIRECTION('ref_axis',(-0.353701527614571,-0.93535834275593,3.5407744807615E-31));
#13704=DIRECTION('center_axis',(0.,0.,1.));
#13705=DIRECTION('ref_axis',(1.,0.,0.));
#13706=DIRECTION('center_axis',(0.,0.,-1.));
#13707=DIRECTION('ref_axis',(-1.,0.,0.));
#13708=DIRECTION('center_axis',(-2.52323414687536E-16,0.,-1.));
#13709=DIRECTION('ref_axis',(-1.,0.,2.52323414687536E-16));
#13710=DIRECTION('center_axis',(-2.52323414687536E-16,0.,-1.));
#13711=DIRECTION('ref_axis',(-1.,0.,2.52323414687536E-16));
#13712=DIRECTION('',(-2.52323414687536E-16,0.,-1.));
#13713=DIRECTION('center_axis',(2.52323414687536E-16,0.,1.));
#13714=DIRECTION('ref_axis',(-1.,4.9737991503207E-14,2.52323414687536E-16));
#13715=DIRECTION('center_axis',(-2.52323414687536E-16,0.,-1.));
#13716=DIRECTION('ref_axis',(-1.,0.,2.52323414687536E-16));
#13717=DIRECTION('center_axis',(-2.52323414687536E-16,0.,-1.));
#13718=DIRECTION('ref_axis',(-1.,0.,2.52323414687536E-16));
#13719=DIRECTION('center_axis',(-2.52323414687536E-16,0.,-1.));
#13720=DIRECTION('ref_axis',(-1.,0.,2.52323414687536E-16));
#13721=DIRECTION('',(0.,-1.,0.));
#13722=DIRECTION('center_axis',(2.52323414687536E-16,0.,1.));
#13723=DIRECTION('ref_axis',(-1.,1.77635683940025E-15,2.52323414687536E-16));
#13724=DIRECTION('center_axis',(-2.52323414687536E-16,0.,-1.));
#13725=DIRECTION('ref_axis',(-1.,0.,2.52323414687536E-16));
#13726=DIRECTION('center_axis',(-2.52323414687536E-16,0.,-1.));
#13727=DIRECTION('ref_axis',(-1.,0.,2.52323414687536E-16));
#13728=DIRECTION('center_axis',(-2.52323414687536E-16,0.,-1.));
#13729=DIRECTION('ref_axis',(-1.,0.,2.52323414687536E-16));
#13730=DIRECTION('center_axis',(-0.0239544909236863,-0.859725218195524,
-0.510194797663838));
#13731=DIRECTION('ref_axis',(0.0142235277005771,0.509996493084021,-0.860058874904359));
#13732=DIRECTION('',(-3.04630100940178E-45,8.57457505675013E-31,-1.));
#13733=DIRECTION('center_axis',(-0.023954490923717,-0.859725218194695,0.510194797665234));
#13734=DIRECTION('ref_axis',(-0.0403411650264477,0.510756839498867,0.858778225917168));
#13735=DIRECTION('center_axis',(2.52323414687536E-16,0.,1.));
#13736=DIRECTION('ref_axis',(-1.,8.88178419700125E-16,2.52323414687536E-16));
#13737=DIRECTION('center_axis',(2.52323414687536E-16,0.,1.));
#13738=DIRECTION('ref_axis',(1.,0.,-2.52323414687536E-16));
#13739=DIRECTION('center_axis',(-2.52323414687536E-16,0.,-1.));
#13740=DIRECTION('ref_axis',(1.,-8.88178419700125E-16,-2.52323414687536E-16));
#13741=DIRECTION('',(0.,1.,0.));
#13742=DIRECTION('center_axis',(2.52323414687536E-16,0.,1.));
#13743=DIRECTION('ref_axis',(1.,0.,-2.52323414687536E-16));
#13744=DIRECTION('center_axis',(2.52323414687536E-16,0.,1.));
#13745=DIRECTION('ref_axis',(1.,0.,-2.52323414687536E-16));
#13746=DIRECTION('center_axis',(2.52323414687536E-16,0.,1.));
#13747=DIRECTION('ref_axis',(1.,0.,-2.52323414687536E-16));
#13748=DIRECTION('center_axis',(3.5527136788005E-15,-1.,-8.57457505675013E-31));
#13749=DIRECTION('ref_axis',(1.,3.5527136788005E-15,0.));
#13750=DIRECTION('center_axis',(3.5527136788005E-15,-1.,-8.57457505675013E-31));
#13751=DIRECTION('ref_axis',(1.,3.5527136788005E-15,-1.26929208725075E-46));
#13752=DIRECTION('',(0.99034174667433,3.51840067009707E-15,-0.138647844534406));
#13753=DIRECTION('',(-0.99034174667433,-3.51840067009707E-15,-0.138647844534406));
#13754=DIRECTION('center_axis',(3.5527136788005E-15,-1.,-8.57457505675013E-31));
#13755=DIRECTION('ref_axis',(1.,3.5527136788005E-15,-1.26929208725075E-46));
#13756=DIRECTION('center_axis',(-0.138647844534406,-4.81031341614835E-16,
-0.99034174667433));
#13757=DIRECTION('ref_axis',(-0.99034174667433,3.0510584428262E-33,0.138647844534406));
#13758=DIRECTION('',(0.9714691757235,0.194293835144703,-0.13600568460129));
#13759=DIRECTION('',(-0.99034174667433,0.,0.138647844534406));
#13760=DIRECTION('',(-6.66939586683906E-17,1.,-4.76385419059932E-16));
#13761=DIRECTION('center_axis',(-0.138647844534408,1.96239838967726E-14,
-0.99034174667433));
#13762=DIRECTION('ref_axis',(-0.142395756615911,0.98960902789351,0.019935405926249));
#13763=DIRECTION('center_axis',(-0.138647844534406,-4.81031341614834E-16,
0.99034174667433));
#13764=DIRECTION('ref_axis',(0.99034174667433,1.28749462997746E-32,0.138647844534406));
#13765=DIRECTION('',(6.66939586683902E-17,-1.,-4.76385419059931E-16));
#13766=DIRECTION('',(0.99034174667433,0.,0.138647844534406));
#13767=DIRECTION('',(-0.9714691757235,-0.194293835144704,-0.13600568460129));
#13768=DIRECTION('center_axis',(-0.138647844534407,4.36088531502231E-15,
0.99034174667433));
#13769=DIRECTION('ref_axis',(-0.192413756189259,0.980944083309111,-0.0269379258665006));
#13770=DIRECTION('center_axis',(-0.196116135138187,0.98058067569092,4.73331845067205E-17));
#13771=DIRECTION('ref_axis',(-0.980580675690919,-0.196116135138187,9.12179048335121E-36));
#13772=DIRECTION('',(-0.9714691757235,-0.194293835144703,0.13600568460129));
#13773=DIRECTION('',(9.28280120924076E-18,-4.6414006046203E-17,1.));
#13774=DIRECTION('',(0.9714691757235,0.194293835144704,0.13600568460129));
#13775=DIRECTION('center_axis',(3.46944695195362E-15,-1.,-8.754227019942E-31));
#13776=DIRECTION('ref_axis',(1.,3.46944695195362E-15,0.));
#13777=DIRECTION('center_axis',(-3.46944695195362E-15,1.,8.754227019942E-31));
#13778=DIRECTION('ref_axis',(1.,3.46944695195362E-15,-5.52224113655355E-47));
#13779=DIRECTION('center_axis',(0.0285016084921434,0.833421796752127,0.551901954165607));
#13780=DIRECTION('ref_axis',(-0.0430076714350775,0.552637411426228,-0.832311379046238));
#13781=DIRECTION('center_axis',(-2.52323414687536E-16,0.,-1.));
#13782=DIRECTION('ref_axis',(-1.,0.,2.52323414687536E-16));
#13783=DIRECTION('center_axis',(0.169336824475723,-4.83683914468181E-13,
-0.985558237688914));
#13784=DIRECTION('ref_axis',(-0.141035172496763,0.989707972370685,-0.0242324069113047));
#13785=DIRECTION('center_axis',(0.169336824475649,-5.71923547513346E-14,
0.985558237688927));
#13786=DIRECTION('ref_axis',(-0.190594454957618,0.981122494345506,0.0327475927155013));
#13787=DIRECTION('center_axis',(2.52323414687536E-16,0.,1.));
#13788=DIRECTION('ref_axis',(-1.,9.71445146547012E-15,2.52323414687536E-16));
#13789=DIRECTION('center_axis',(-2.52323414687536E-16,0.,-1.));
#13790=DIRECTION('ref_axis',(-1.,0.,2.52323414687536E-16));
#13791=DIRECTION('center_axis',(-3.46944695195361E-15,1.,8.75422701994197E-31));
#13792=DIRECTION('ref_axis',(-1.,-3.46944695195361E-15,6.22301527786114E-61));
#13793=DIRECTION('center_axis',(0.0285016084921437,0.833421796752069,-0.551901954165695));
#13794=DIRECTION('ref_axis',(0.0188743829595763,0.551579119228361,0.83390900756567));
#13795=DIRECTION('center_axis',(-3.46944695195361E-15,1.,8.75422701994197E-31));
#13796=DIRECTION('ref_axis',(-1.,-3.46944695195361E-15,5.52224113655467E-47));
#13797=DIRECTION('center_axis',(-0.9714691757235,-0.194293835144704,-0.13600568460129));
#13798=DIRECTION('ref_axis',(0.196116135138187,-0.980580675690919,1.08828652437483E-18));
#13799=DIRECTION('center_axis',(0.971469175723501,0.194293835144703,0.13600568460129));
#13800=DIRECTION('ref_axis',(-0.196116135138187,0.98058067569092,-1.50980502241592E-17));
#13801=DIRECTION('center_axis',(0.980051041638971,0.143785099769423,0.137207145829456));
#13802=DIRECTION('ref_axis',(-0.145157949036735,0.989408494925856,-5.6122374695011E-17));
#13803=DIRECTION('center_axis',(0.999978809045156,0.00651010450232907,-2.52318067713449E-16));
#13804=DIRECTION('ref_axis',(-0.00651010450232907,0.999978809045156,-1.80918359374754E-32));
#13805=DIRECTION('center_axis',(2.52323414687536E-16,0.,1.));
#13806=DIRECTION('ref_axis',(1.,0.,-2.66453525910038E-16));
#13807=DIRECTION('center_axis',(0.994514519537326,-0.104598615810349,-2.50939299525992E-16));
#13808=DIRECTION('ref_axis',(0.104598615810349,0.994514519537326,-1.52162986309358E-32));
#13809=DIRECTION('center_axis',(2.52323414687536E-16,0.,1.));
#13810=DIRECTION('ref_axis',(1.,0.,-2.41886888769396E-16));
#13811=DIRECTION('center_axis',(-0.9714691757235,-0.194293835144704,0.13600568460129));
#13812=DIRECTION('ref_axis',(0.196116135138187,-0.980580675690919,-3.35108818532205E-18));
#13813=DIRECTION('center_axis',(0.9714691757235,0.194293835144703,-0.13600568460129));
#13814=DIRECTION('ref_axis',(0.196116135138188,-0.980580675690919,3.62636123721662E-15));
#13815=DIRECTION('center_axis',(0.980051041638971,0.143785099769423,-0.137207145829457));
#13816=DIRECTION('ref_axis',(-0.145157949036735,0.989408494925857,2.8694747315233E-18));
#13817=DIRECTION('center_axis',(0.999978809045156,0.00651010450232831,-2.52318067713449E-16));
#13818=DIRECTION('ref_axis',(0.0065101045023283,-0.999978809045156,7.13181002470613E-32));
#13819=DIRECTION('center_axis',(-2.52323414687536E-16,0.,-1.));
#13820=DIRECTION('ref_axis',(-1.,0.,2.66453525910038E-16));
#13821=DIRECTION('center_axis',(0.994514519537326,-0.104598615810349,-2.50939299525992E-16));
#13822=DIRECTION('ref_axis',(-0.104598615810349,-0.994514519537326,4.29233327314378E-32));
#13823=DIRECTION('center_axis',(-2.52323414687536E-16,0.,-1.));
#13824=DIRECTION('ref_axis',(-1.,0.,2.41886888769396E-16));
#13825=DIRECTION('center_axis',(-0.99034174667433,-3.51840067009707E-15,
-0.138647844534406));
#13826=DIRECTION('ref_axis',(-0.138647844534406,-3.26527751285154E-32,0.99034174667433));
#13827=DIRECTION('center_axis',(0.99034174667433,3.51840067009707E-15,0.138647844534406));
#13828=DIRECTION('ref_axis',(0.138647844534406,8.65196281794793E-31,-0.99034174667433));
#13829=DIRECTION('center_axis',(3.5527136788005E-15,-1.,-8.57457505675013E-31));
#13830=DIRECTION('ref_axis',(1.,3.5527136788005E-15,0.));
#13831=DIRECTION('center_axis',(0.998667820387802,3.38652769649194E-15,
0.0516002376145362));
#13832=DIRECTION('ref_axis',(0.0516002376145362,-4.34329619623291E-31,-0.998667820387802));
#13833=DIRECTION('center_axis',(0.999611719795952,-0.0278641283118464,-2.52225442500595E-16));
#13834=DIRECTION('ref_axis',(0.0278641283118464,0.999611719795952,-7.27443156916003E-33));
#13835=DIRECTION('center_axis',(2.52323414687536E-16,0.,1.));
#13836=DIRECTION('ref_axis',(1.,0.,-2.58379176640036E-16));
#13837=DIRECTION('center_axis',(-0.99034174667433,-3.51840067009707E-15,
0.138647844534406));
#13838=DIRECTION('ref_axis',(0.138647844534406,1.9494291318743E-31,0.99034174667433));
#13839=DIRECTION('center_axis',(0.99034174667433,3.51840067009707E-15,-0.138647844534406));
#13840=DIRECTION('ref_axis',(0.138647844534406,2.22044604925031E-15,0.99034174667433));
#13841=DIRECTION('center_axis',(3.5527136788005E-15,-1.,-8.57457505675013E-31));
#13842=DIRECTION('ref_axis',(1.,3.5527136788005E-15,0.));
#13843=DIRECTION('center_axis',(0.998667820387802,3.42216846262747E-15,
-0.0516002376145377));
#13844=DIRECTION('ref_axis',(0.0516002376145376,8.88178419700125E-15,0.998667820387802));
#13845=DIRECTION('center_axis',(0.999611719795952,-0.0278641283118467,-2.52225442500595E-16));
#13846=DIRECTION('ref_axis',(-0.0278641283118467,-0.999611719795952,-6.03275671091393E-32));
#13847=DIRECTION('center_axis',(-2.52323414687536E-16,0.,-1.));
#13848=DIRECTION('ref_axis',(-1.,0.,2.58379176640036E-16));
#13849=DIRECTION('center_axis',(0.935358342755929,-0.353701527614572,-2.3601281100065E-16));
#13850=DIRECTION('ref_axis',(-0.353701527614572,-0.935358342755929,-4.5752724171616E-32));
#13851=DIRECTION('center_axis',(-2.52323414687536E-16,0.,-1.));
#13852=DIRECTION('ref_axis',(-1.,0.,2.03012210217171E-16));
#13853=DIRECTION('center_axis',(0.996895904609183,0.0787309048178609,-2.7669419661291E-16));
#13854=DIRECTION('ref_axis',(-0.0787309048178609,0.996895904609183,1.10831582297851E-32));
#13855=DIRECTION('center_axis',(-0.996895904609183,-0.0787309048178616,
2.51540178739009E-16));
#13856=DIRECTION('ref_axis',(-0.0787309048178616,0.996895904609183,9.57629751275587E-34));
#13857=DIRECTION('center_axis',(2.52323414687536E-16,0.,1.));
#13858=DIRECTION('ref_axis',(1.,0.,-2.03012210217171E-16));
#13859=DIRECTION('center_axis',(-0.93535834275593,0.353701527614571,0.));
#13860=DIRECTION('ref_axis',(-0.353701527614571,-0.93535834275593,0.));
#13861=DIRECTION('center_axis',(1.,0.,0.));
#13862=DIRECTION('ref_axis',(0.,0.,-1.));
#13863=DIRECTION('',(0.,0.,-1.));
#13864=DIRECTION('',(0.,1.,0.));
#13865=DIRECTION('',(0.,0.,1.));
#13866=DIRECTION('',(0.,-1.,0.));
#13867=DIRECTION('center_axis',(0.,-1.,0.));
#13868=DIRECTION('ref_axis',(0.,0.,-1.));
#13869=DIRECTION('',(-1.,0.,0.));
#13870=DIRECTION('',(0.,0.,-1.));
#13871=DIRECTION('',(1.,0.,0.));
#13872=DIRECTION('',(0.707106781186548,0.,0.707106781186548));
#13873=DIRECTION('',(0.,0.,1.));
#13874=DIRECTION('',(-0.707106781186547,0.,0.707106781186547));
#13875=DIRECTION('center_axis',(0.,0.,1.));
#13876=DIRECTION('ref_axis',(1.,0.,0.));
#13877=DIRECTION('',(1.,0.,0.));
#13878=DIRECTION('',(0.,1.,0.));
#13879=DIRECTION('',(-1.,0.,0.));
#13880=DIRECTION('center_axis',(0.,0.,-1.));
#13881=DIRECTION('ref_axis',(1.,0.,0.));
#13882=DIRECTION('center_axis',(0.,0.,1.));
#13883=DIRECTION('ref_axis',(1.,0.,0.));
#13884=DIRECTION('',(-1.,0.,0.));
#13885=DIRECTION('center_axis',(0.,0.,1.));
#13886=DIRECTION('ref_axis',(1.,0.,0.));
#13887=DIRECTION('',(1.,0.,0.));
#13888=DIRECTION('',(0.,-1.,0.));
#13889=DIRECTION('center_axis',(-1.,0.,0.));
#13890=DIRECTION('ref_axis',(0.,0.,1.));
#13891=DIRECTION('',(0.,1.,0.));
#13892=DIRECTION('',(0.,0.,1.));
#13893=DIRECTION('',(0.,-1.,0.));
#13894=DIRECTION('',(0.,0.,-1.));
#13895=DIRECTION('center_axis',(0.,0.,1.));
#13896=DIRECTION('ref_axis',(1.,0.,0.));
#13897=DIRECTION('',(-1.,0.,0.));
#13898=DIRECTION('center_axis',(0.,0.,1.));
#13899=DIRECTION('ref_axis',(1.,0.,0.));
#13900=DIRECTION('',(0.,-1.,0.));
#13901=DIRECTION('center_axis',(0.,0.,1.));
#13902=DIRECTION('ref_axis',(1.,0.,0.));
#13903=DIRECTION('',(0.,1.,0.));
#13904=DIRECTION('center_axis',(0.,0.,-1.));
#13905=DIRECTION('ref_axis',(1.,0.,0.));
#13906=DIRECTION('',(1.,0.,0.));
#13907=DIRECTION('center_axis',(1.,0.,0.));
#13908=DIRECTION('ref_axis',(0.,0.,-1.));
#13909=DIRECTION('',(0.,1.,0.));
#13910=DIRECTION('',(0.,0.,1.));
#13911=DIRECTION('',(0.,-1.,0.));
#13912=DIRECTION('',(0.,0.,-1.));
#13913=DIRECTION('center_axis',(0.,0.,-1.));
#13914=DIRECTION('ref_axis',(1.,0.,0.));
#13915=DIRECTION('',(0.,1.,0.));
#13916=DIRECTION('center_axis',(0.,0.,-1.));
#13917=DIRECTION('ref_axis',(-1.,0.,0.));
#13918=DIRECTION('',(1.,0.,0.));
#13919=DIRECTION('center_axis',(0.,0.,-1.));
#13920=DIRECTION('ref_axis',(1.,0.,0.));
#13921=DIRECTION('',(-1.,0.,0.));
#13922=DIRECTION('center_axis',(0.,0.,1.));
#13923=DIRECTION('ref_axis',(-1.,-4.44089209850063E-15,0.));
#13924=DIRECTION('',(0.,-1.,0.));
#13925=DIRECTION('center_axis',(1.,0.,0.));
#13926=DIRECTION('ref_axis',(0.,0.,-1.));
#13927=DIRECTION('',(0.,0.,-1.));
#13928=DIRECTION('',(0.,-1.,0.));
#13929=DIRECTION('',(0.,0.,1.));
#13930=DIRECTION('',(0.,1.,0.));
#13931=DIRECTION('center_axis',(0.,0.,1.));
#13932=DIRECTION('ref_axis',(-1.,0.,0.));
#13933=DIRECTION('',(0.,-1.,0.));
#13934=DIRECTION('',(1.,0.,0.));
#13935=DIRECTION('center_axis',(0.,0.,-1.));
#13936=DIRECTION('ref_axis',(1.,1.06581410364015E-14,0.));
#13937=DIRECTION('',(-1.,0.,0.));
#13938=DIRECTION('center_axis',(0.,0.,1.));
#13939=DIRECTION('ref_axis',(-1.,0.,0.));
#13940=DIRECTION('',(1.,0.,0.));
#13941=DIRECTION('center_axis',(0.,0.,1.));
#13942=DIRECTION('ref_axis',(1.,0.,0.));
#13943=DIRECTION('',(-1.,0.,0.));
#13944=DIRECTION('',(0.,1.,0.));
#13945=DIRECTION('center_axis',(-1.,0.,0.));
#13946=DIRECTION('ref_axis',(0.,0.,1.));
#13947=DIRECTION('',(0.,0.,1.));
#13948=DIRECTION('',(0.,1.,0.));
#13949=DIRECTION('',(0.,0.,-1.));
#13950=DIRECTION('',(0.,-1.,0.));
#13951=DIRECTION('center_axis',(0.,0.,1.));
#13952=DIRECTION('ref_axis',(-1.,0.,0.));
#13953=DIRECTION('',(0.,1.,0.));
#13954=DIRECTION('center_axis',(0.,0.,1.));
#13955=DIRECTION('ref_axis',(1.,0.,0.));
#13956=DIRECTION('',(-1.,0.,0.));
#13957=DIRECTION('center_axis',(0.,0.,1.));
#13958=DIRECTION('ref_axis',(-1.,0.,0.));
#13959=DIRECTION('',(1.,0.,0.));
#13960=DIRECTION('center_axis',(0.,0.,-1.));
#13961=DIRECTION('ref_axis',(1.,-4.44089209850063E-15,0.));
#13962=DIRECTION('',(0.,-1.,0.));
#13963=DIRECTION('center_axis',(1.,0.,0.));
#13964=DIRECTION('ref_axis',(0.,0.,-1.));
#13965=DIRECTION('',(0.,0.,1.));
#13966=DIRECTION('',(0.,1.,0.));
#13967=DIRECTION('',(0.,0.,-1.));
#13968=DIRECTION('',(0.,-1.,0.));
#13969=DIRECTION('center_axis',(0.,0.,-1.));
#13970=DIRECTION('ref_axis',(-1.,0.,0.));
#13971=DIRECTION('',(1.,0.,0.));
#13972=DIRECTION('center_axis',(0.,0.,-1.));
#13973=DIRECTION('ref_axis',(-1.,0.,0.));
#13974=DIRECTION('',(0.,-1.,0.));
#13975=DIRECTION('center_axis',(0.,0.,-1.));
#13976=DIRECTION('ref_axis',(-1.,0.,0.));
#13977=DIRECTION('',(0.,1.,0.));
#13978=DIRECTION('center_axis',(0.,0.,1.));
#13979=DIRECTION('ref_axis',(-1.,0.,0.));
#13980=DIRECTION('',(-1.,0.,0.));
#13981=DIRECTION('center_axis',(-0.707106781186548,0.,0.707106781186548));
#13982=DIRECTION('ref_axis',(0.,1.,0.));
#13983=DIRECTION('',(-0.707106781186547,0.,-0.707106781186547));
#13984=DIRECTION('',(0.,-1.,0.));
#13985=DIRECTION('',(0.707106781186547,0.,0.707106781186547));
#13986=DIRECTION('',(0.,1.,0.));
#13987=DIRECTION('center_axis',(0.707106781186548,0.,0.707106781186548));
#13988=DIRECTION('ref_axis',(0.,-1.,0.));
#13989=DIRECTION('',(0.707106781186547,0.,-0.707106781186547));
#13990=DIRECTION('',(0.,-1.,0.));
#13991=DIRECTION('',(-0.707106781186547,0.,0.707106781186547));
#13992=DIRECTION('',(0.,1.,0.));
#13993=DIRECTION('center_axis',(-0.707106781186548,0.,-0.707106781186548));
#13994=DIRECTION('ref_axis',(0.,-1.,0.));
#13995=DIRECTION('',(0.707106781186547,0.,-0.707106781186547));
#13996=DIRECTION('',(0.,1.,0.));
#13997=DIRECTION('',(-0.707106781186547,0.,0.707106781186547));
#13998=DIRECTION('',(0.,-1.,0.));
#13999=DIRECTION('center_axis',(0.707106781186548,0.,-0.707106781186548));
#14000=DIRECTION('ref_axis',(0.,1.,0.));
#14001=DIRECTION('',(0.,-1.,0.));
#14002=DIRECTION('',(-0.707106781186547,0.,-0.707106781186547));
#14003=DIRECTION('',(0.,1.,0.));
#14004=DIRECTION('',(0.707106781186547,0.,0.707106781186547));
#14005=DIRECTION('center_axis',(0.,0.,1.));
#14006=DIRECTION('ref_axis',(1.,0.,0.));
#14007=DIRECTION('center_axis',(0.,0.,1.));
#14008=DIRECTION('ref_axis',(1.,0.,0.));
#14009=DIRECTION('center_axis',(1.,0.,0.));
#14010=DIRECTION('ref_axis',(0.,0.,-1.));
#14011=DIRECTION('center_axis',(1.,0.,0.));
#14012=DIRECTION('ref_axis',(0.,0.,-1.));
#14013=DIRECTION('center_axis',(0.,1.,0.));
#14014=DIRECTION('ref_axis',(0.,0.,1.));
#14015=DIRECTION('center_axis',(0.,-1.,0.));
#14016=DIRECTION('ref_axis',(0.,0.,-1.));
#14017=DIRECTION('center_axis',(0.,0.,1.));
#14018=DIRECTION('ref_axis',(1.,0.,0.));
#14019=DIRECTION('center_axis',(0.518508516521689,-0.855072463768117,-4.74660568499161E-15));
#14020=DIRECTION('ref_axis',(0.855072463768117,0.518508516521689,-1.27467223778887E-31));
#14021=DIRECTION('center_axis',(0.,1.,0.));
#14022=DIRECTION('ref_axis',(1.,0.,0.));
#14023=DIRECTION('center_axis',(0.,1.,0.));
#14024=DIRECTION('ref_axis',(1.11022302462516E-14,0.,-1.));
#14025=DIRECTION('center_axis',(0.707106781186545,3.92523114670951E-15,
-0.70710678118655));
#14026=DIRECTION('ref_axis',(0.70710678118655,9.38409251374148E-32,0.707106781186545));
#14027=DIRECTION('center_axis',(1.66533453693773E-14,0.,1.));
#14028=DIRECTION('ref_axis',(-1.,0.,1.66533453693773E-14));
#14029=DIRECTION('center_axis',(0.,1.,0.));
#14030=DIRECTION('ref_axis',(1.,0.,0.));
#14031=DIRECTION('center_axis',(-0.707106781186545,-1.17756934401283E-14,
0.70710678118655));
#14032=DIRECTION('ref_axis',(-0.70710678118655,-2.63935455544261E-31,-0.707106781186545));
#14033=DIRECTION('center_axis',(1.,0.,1.11022302462516E-14));
#14034=DIRECTION('ref_axis',(-1.11022302462516E-14,0.,1.));
#14035=DIRECTION('center_axis',(0.,-1.,0.));
#14036=DIRECTION('ref_axis',(-1.11022302462516E-14,0.,1.));
#14037=DIRECTION('center_axis',(0.,-1.,0.));
#14038=DIRECTION('ref_axis',(0.,0.,-1.));
#14039=DIRECTION('center_axis',(0.,0.,-1.));
#14040=DIRECTION('ref_axis',(1.,0.,0.));
#14041=DIRECTION('center_axis',(0.,0.,-1.));
#14042=DIRECTION('ref_axis',(1.,0.,0.));
#14043=DIRECTION('center_axis',(0.,0.,-1.));
#14044=DIRECTION('ref_axis',(0.924701283533291,-0.380693493813441,0.));
#14045=DIRECTION('center_axis',(0.,0.,1.));
#14046=DIRECTION('ref_axis',(1.,0.,0.));
#14047=DIRECTION('center_axis',(-1.,0.,0.));
#14048=DIRECTION('ref_axis',(0.,0.,1.));
#14049=DIRECTION('center_axis',(0.,1.,0.));
#14050=DIRECTION('ref_axis',(0.,0.,1.));
#14051=DIRECTION('center_axis',(0.,-1.,0.));
#14052=DIRECTION('ref_axis',(0.,0.,-1.));
#14053=DIRECTION('center_axis',(0.707106781186548,0.,-0.707106781186548));
#14054=DIRECTION('ref_axis',(-0.707106781186548,0.,-0.707106781186548));
#14055=DIRECTION('center_axis',(0.707106781186564,0.,-0.707106781186531));
#14056=DIRECTION('ref_axis',(-0.707106781186531,0.,-0.707106781186564));
#14057=DIRECTION('center_axis',(0.,0.,-1.));
#14058=DIRECTION('ref_axis',(-1.,0.,0.));
#14059=DIRECTION('center_axis',(0.,-5.55111512312578E-15,1.));
#14060=DIRECTION('ref_axis',(0.,-1.,-5.55111512312578E-15));
#14061=DIRECTION('center_axis',(0.,-1.,0.));
#14062=DIRECTION('ref_axis',(0.,0.,-1.));
#14063=DIRECTION('center_axis',(0.,1.,0.));
#14064=DIRECTION('ref_axis',(0.,0.,1.));
#14065=DIRECTION('center_axis',(-0.707106781186548,0.,0.707106781186548));
#14066=DIRECTION('ref_axis',(0.707106781186548,0.,0.707106781186548));
#14067=DIRECTION('center_axis',(-0.707106781186553,0.,0.707106781186542));
#14068=DIRECTION('ref_axis',(0.707106781186542,0.,0.707106781186553));
#14069=DIRECTION('center_axis',(0.,0.,1.));
#14070=DIRECTION('ref_axis',(1.,0.,0.));
#14071=DIRECTION('center_axis',(0.,0.,-1.));
#14072=DIRECTION('ref_axis',(-1.,0.,0.));
#14073=DIRECTION('center_axis',(0.,-1.,0.));
#14074=DIRECTION('ref_axis',(0.,0.,-1.));
#14075=DIRECTION('center_axis',(0.,-1.,0.));
#14076=DIRECTION('ref_axis',(0.,0.,-1.));
#14077=DIRECTION('center_axis',(0.,0.,-1.));
#14078=DIRECTION('ref_axis',(-1.,0.,0.));
#14079=DIRECTION('center_axis',(0.,0.,-1.));
#14080=DIRECTION('ref_axis',(-1.,0.,0.));
#14081=DIRECTION('center_axis',(-0.739130434782608,0.673562321079551,0.));
#14082=DIRECTION('ref_axis',(0.673562321079551,0.739130434782608,0.));
#14083=DIRECTION('center_axis',(0.,1.,0.));
#14084=DIRECTION('ref_axis',(1.,0.,0.));
#14085=DIRECTION('center_axis',(1.,-3.33066907387547E-14,0.));
#14086=DIRECTION('ref_axis',(-3.33066907387547E-14,-1.,0.));
#14087=DIRECTION('center_axis',(0.,1.,0.));
#14088=DIRECTION('ref_axis',(1.,0.,0.));
#14089=DIRECTION('center_axis',(0.,1.,0.));
#14090=DIRECTION('ref_axis',(0.,0.,-1.));
#14091=DIRECTION('center_axis',(0.707106781186548,0.,0.707106781186548));
#14092=DIRECTION('ref_axis',(-0.707106781186548,0.,0.707106781186548));
#14093=DIRECTION('center_axis',(0.,1.,0.));
#14094=DIRECTION('ref_axis',(1.,0.,0.));
#14095=DIRECTION('center_axis',(0.,-5.55111512312578E-15,1.));
#14096=DIRECTION('ref_axis',(0.,1.,5.55111512312578E-15));
#14097=DIRECTION('center_axis',(0.,-1.,0.));
#14098=DIRECTION('ref_axis',(0.,0.,-1.));
#14099=DIRECTION('center_axis',(-1.,0.,0.));
#14100=DIRECTION('ref_axis',(0.,0.,-1.));
#14101=DIRECTION('center_axis',(-0.518508516521692,0.855072463768115,0.));
#14102=DIRECTION('ref_axis',(0.855072463768115,0.518508516521692,-5.55111512312579E-15));
#14103=DIRECTION('center_axis',(0.,0.,1.));
#14104=DIRECTION('ref_axis',(1.,0.,0.));
#14105=DIRECTION('center_axis',(-0.797101449275362,0.603845410318832,0.));
#14106=DIRECTION('ref_axis',(-0.603845410318832,-0.797101449275361,0.));
#14107=DIRECTION('center_axis',(1.,0.,0.));
#14108=DIRECTION('ref_axis',(0.,0.,-1.));
#14109=DIRECTION('center_axis',(0.707106781186548,0.,0.707106781186548));
#14110=DIRECTION('ref_axis',(0.707106781186548,0.,-0.707106781186548));
#14111=DIRECTION('center_axis',(0.707106781186545,-3.92523114670945E-15,
0.70710678118655));
#14112=DIRECTION('ref_axis',(0.70710678118655,3.86675578882201E-31,-0.707106781186545));
#14113=DIRECTION('center_axis',(0.,-1.,0.));
#14114=DIRECTION('ref_axis',(0.,0.,-1.));
#14115=DIRECTION('center_axis',(0.,1.,0.));
#14116=DIRECTION('ref_axis',(0.,0.,1.));
#14117=DIRECTION('center_axis',(0.,0.,-1.));
#14118=DIRECTION('ref_axis',(-1.,0.,0.));
#14119=DIRECTION('center_axis',(-5.55111512312578E-15,0.,1.));
#14120=DIRECTION('ref_axis',(1.,0.,5.55111512312578E-15));
#14121=DIRECTION('center_axis',(-1.,0.,0.));
#14122=DIRECTION('ref_axis',(0.,0.,1.));
#14123=DIRECTION('center_axis',(0.,0.,1.));
#14124=DIRECTION('ref_axis',(1.,0.,0.));
#14125=DIRECTION('center_axis',(0.,0.,-1.));
#14126=DIRECTION('ref_axis',(1.,0.,0.));
#14127=DIRECTION('center_axis',(0.,1.,0.));
#14128=DIRECTION('ref_axis',(1.,0.,0.));
#14129=DIRECTION('center_axis',(0.,1.,0.));
#14130=DIRECTION('ref_axis',(1.11022302462516E-14,0.,-1.));
#14131=DIRECTION('center_axis',(1.,0.,1.11022302462516E-14));
#14132=DIRECTION('ref_axis',(-1.11022302462516E-14,0.,1.));
#14133=DIRECTION('center_axis',(0.,1.,0.));
#14134=DIRECTION('ref_axis',(1.,0.,0.));
#14135=DIRECTION('center_axis',(0.707106781186545,-3.92523114670945E-15,
0.70710678118655));
#14136=DIRECTION('ref_axis',(-0.70710678118655,-3.86675578882201E-31,0.707106781186545));
#14137=DIRECTION('center_axis',(0.,0.,-1.));
#14138=DIRECTION('ref_axis',(-1.,0.,0.));
#14139=DIRECTION('center_axis',(0.,0.,-1.));
#14140=DIRECTION('ref_axis',(-1.,0.,0.));
#14141=DIRECTION('center_axis',(-1.,0.,0.));
#14142=DIRECTION('ref_axis',(0.,0.,1.));
#14143=DIRECTION('center_axis',(0.,-1.,0.));
#14144=DIRECTION('ref_axis',(0.,0.,-1.));
#14145=DIRECTION('center_axis',(0.,1.,0.));
#14146=DIRECTION('ref_axis',(0.,0.,1.));
#14147=DIRECTION('center_axis',(-0.707106781186548,0.,-0.707106781186548));
#14148=DIRECTION('ref_axis',(-0.707106781186548,0.,0.707106781186548));
#14149=DIRECTION('center_axis',(0.707106781186553,0.,0.707106781186542));
#14150=DIRECTION('ref_axis',(0.707106781186542,0.,-0.707106781186553));
#14151=DIRECTION('center_axis',(-1.,0.,0.));
#14152=DIRECTION('ref_axis',(0.,0.,1.));
#14153=DIRECTION('center_axis',(1.,0.,0.));
#14154=DIRECTION('ref_axis',(0.,0.,-1.));
#14155=DIRECTION('center_axis',(0.,0.,-1.));
#14156=DIRECTION('ref_axis',(0.924701283533291,-0.380693493813441,0.));
#14157=DIRECTION('center_axis',(0.797101449275362,-0.603845410318832,0.));
#14158=DIRECTION('ref_axis',(-0.603845410318832,-0.797101449275361,0.));
#14159=DIRECTION('center_axis',(0.,1.,0.));
#14160=DIRECTION('ref_axis',(1.,0.,0.));
#14161=DIRECTION('center_axis',(1.,0.,0.));
#14162=DIRECTION('ref_axis',(0.,0.,1.));
#14163=DIRECTION('center_axis',(0.,-1.,0.));
#14164=DIRECTION('ref_axis',(0.,0.,-1.));
#14165=DIRECTION('center_axis',(0.,0.,-1.));
#14166=DIRECTION('ref_axis',(1.,0.,0.));
#14167=DIRECTION('center_axis',(0.,1.,0.));
#14168=DIRECTION('ref_axis',(0.,0.,-1.));
#14169=DIRECTION('center_axis',(0.,0.,1.));
#14170=DIRECTION('ref_axis',(1.,0.,0.));
#14171=DIRECTION('center_axis',(0.739130434782608,-0.673562321079551,0.));
#14172=DIRECTION('ref_axis',(0.673562321079551,0.739130434782608,0.));
#14173=DIRECTION('center_axis',(1.,0.,0.));
#14174=DIRECTION('ref_axis',(0.,0.,-1.));
#14175=DIRECTION('center_axis',(0.,0.,1.));
#14176=DIRECTION('ref_axis',(1.,0.,0.));
#14177=DIRECTION('center_axis',(0.,0.,-1.));
#14178=DIRECTION('ref_axis',(-1.,0.,0.));
#14179=DIRECTION('center_axis',(0.,1.,0.));
#14180=DIRECTION('ref_axis',(0.,0.,1.));
#14181=DIRECTION('center_axis',(0.,0.,-1.));
#14182=DIRECTION('ref_axis',(-1.,0.,0.));
#14183=DIRECTION('center_axis',(0.518508516521689,-0.855072463768117,-4.74660568499161E-15));
#14184=DIRECTION('ref_axis',(0.855072463768117,0.518508516521689,-1.27467223778887E-31));
#14185=DIRECTION('center_axis',(0.,0.,1.));
#14186=DIRECTION('ref_axis',(-1.,0.,0.));
#14187=DIRECTION('center_axis',(0.,-1.,0.));
#14188=DIRECTION('ref_axis',(0.,0.,-1.));
#14189=DIRECTION('center_axis',(-1.,0.,0.));
#14190=DIRECTION('ref_axis',(0.,0.,-1.));
#14191=DIRECTION('center_axis',(0.,1.,0.));
#14192=DIRECTION('ref_axis',(0.,0.,-1.));
#14193=DIRECTION('center_axis',(0.,0.,-1.));
#14194=DIRECTION('ref_axis',(1.,0.,0.));
#14195=DIRECTION('center_axis',(0.,0.,-1.));
#14196=DIRECTION('ref_axis',(0.924701283533291,-0.380693493813441,0.));
#14197=DIRECTION('center_axis',(1.,0.,0.));
#14198=DIRECTION('ref_axis',(0.,0.,-1.));
#14199=DIRECTION('center_axis',(0.,-1.,0.));
#14200=DIRECTION('ref_axis',(0.,0.,-1.));
#14201=DIRECTION('center_axis',(0.,0.,-1.));
#14202=DIRECTION('ref_axis',(-1.,0.,0.));
#14203=DIRECTION('center_axis',(0.,0.,-1.));
#14204=DIRECTION('ref_axis',(-1.,0.,0.));
#14205=DIRECTION('center_axis',(-0.518508516521693,0.855072463768114,0.));
#14206=DIRECTION('ref_axis',(0.855072463768114,0.518508516521693,0.));
#14207=DIRECTION('center_axis',(0.,0.,-1.));
#14208=DIRECTION('ref_axis',(-1.,0.,0.));
#14209=DIRECTION('center_axis',(0.,1.,0.));
#14210=DIRECTION('ref_axis',(1.,0.,0.));
#14211=DIRECTION('center_axis',(-0.707106781186559,0.,-0.707106781186536));
#14212=DIRECTION('ref_axis',(0.707106781186536,0.,-0.707106781186559));
#14213=DIRECTION('center_axis',(0.,1.,0.));
#14214=DIRECTION('ref_axis',(0.,0.,-1.));
#14215=DIRECTION('center_axis',(0.,1.11022302462516E-14,1.));
#14216=DIRECTION('ref_axis',(0.,1.,-1.11022302462516E-14));
#14217=DIRECTION('center_axis',(-0.707106781186548,0.,-0.707106781186548));
#14218=DIRECTION('ref_axis',(-0.707106781186548,0.,0.707106781186548));
#14219=DIRECTION('center_axis',(0.707106781186545,-3.92523114670939E-15,
0.70710678118655));
#14220=DIRECTION('ref_axis',(0.70710678118655,-2.00573270066562E-31,-0.707106781186545));
#14221=DIRECTION('center_axis',(-0.707106781186559,0.,-0.707106781186536));
#14222=DIRECTION('ref_axis',(-0.707106781186536,0.,0.707106781186559));
#14223=DIRECTION('center_axis',(0.,1.,0.));
#14224=DIRECTION('ref_axis',(0.,0.,1.));
#14225=DIRECTION('center_axis',(0.,1.,0.));
#14226=DIRECTION('ref_axis',(0.,0.,1.));
#14227=DIRECTION('center_axis',(0.,0.,-1.));
#14228=DIRECTION('ref_axis',(-1.,0.,0.));
#14229=DIRECTION('center_axis',(0.,0.,1.));
#14230=DIRECTION('ref_axis',(1.,0.,0.));
#14231=DIRECTION('center_axis',(0.707106781186548,0.,0.707106781186548));
#14232=DIRECTION('ref_axis',(0.707106781186548,0.,-0.707106781186548));
#14233=DIRECTION('center_axis',(-0.707106781186545,-3.92523114670945E-15,
-0.70710678118655));
#14234=DIRECTION('ref_axis',(-0.70710678118655,3.86675578882201E-31,0.707106781186545));
#14235=DIRECTION('center_axis',(0.,1.,0.));
#14236=DIRECTION('ref_axis',(0.,0.,1.));
#14237=DIRECTION('center_axis',(0.,1.,0.));
#14238=DIRECTION('ref_axis',(0.,0.,1.));
#14239=DIRECTION('center_axis',(0.,-1.,0.));
#14240=DIRECTION('ref_axis',(0.,0.,-1.));
#14241=DIRECTION('center_axis',(0.,1.,0.));
#14242=DIRECTION('ref_axis',(1.,0.,0.));
#14243=DIRECTION('center_axis',(-1.,1.11022302462516E-14,0.));
#14244=DIRECTION('ref_axis',(1.11022302462516E-14,1.,0.));
#14245=DIRECTION('center_axis',(0.,1.,0.));
#14246=DIRECTION('ref_axis',(1.,0.,0.));
#14247=DIRECTION('center_axis',(-1.11022302462516E-14,0.,1.));
#14248=DIRECTION('ref_axis',(-1.,0.,-1.11022302462516E-14));
#14249=DIRECTION('center_axis',(0.,1.,0.));
#14250=DIRECTION('ref_axis',(1.,0.,0.));
#14251=DIRECTION('center_axis',(-0.707106781186545,0.,0.70710678118655));
#14252=DIRECTION('ref_axis',(-0.70710678118655,0.,-0.707106781186545));
#14253=DIRECTION('center_axis',(0.,1.,0.));
#14254=DIRECTION('ref_axis',(0.,0.,-1.));
#14255=DIRECTION('center_axis',(0.,1.,0.));
#14256=DIRECTION('ref_axis',(1.,0.,0.));
#14257=DIRECTION('center_axis',(-1.,0.,-1.11022302462516E-14));
#14258=DIRECTION('ref_axis',(1.11022302462516E-14,0.,-1.));
#14259=DIRECTION('center_axis',(-1.,0.,0.));
#14260=DIRECTION('ref_axis',(0.,0.,1.));
#14261=DIRECTION('center_axis',(0.,0.,-1.));
#14262=DIRECTION('ref_axis',(-1.,0.,0.));
#14263=DIRECTION('center_axis',(0.,-1.11022302462516E-14,1.));
#14264=DIRECTION('ref_axis',(0.,-1.,-1.11022302462516E-14));
#14265=DIRECTION('center_axis',(0.,1.,0.));
#14266=DIRECTION('ref_axis',(0.,0.,1.));
#14267=DIRECTION('center_axis',(0.,1.,0.));
#14268=DIRECTION('ref_axis',(0.,0.,1.));
#14269=DIRECTION('center_axis',(0.707106781186548,0.,-0.707106781186548));
#14270=DIRECTION('ref_axis',(-0.707106781186548,0.,-0.707106781186548));
#14271=DIRECTION('center_axis',(-0.707106781186553,0.,0.707106781186542));
#14272=DIRECTION('ref_axis',(0.707106781186542,0.,0.707106781186553));
#14273=DIRECTION('center_axis',(1.,0.,0.));
#14274=DIRECTION('ref_axis',(0.,0.,-1.));
#14275=DIRECTION('center_axis',(0.,0.,1.));
#14276=DIRECTION('ref_axis',(1.,0.,0.));
#14277=DIRECTION('center_axis',(0.797101449275362,0.603845410318832,0.));
#14278=DIRECTION('ref_axis',(-0.603845410318832,0.797101449275361,0.));
#14279=DIRECTION('center_axis',(-0.739130434782608,-0.673562321079551,0.));
#14280=DIRECTION('ref_axis',(0.673562321079551,-0.739130434782608,0.));
#14281=DIRECTION('center_axis',(0.,1.,0.));
#14282=DIRECTION('ref_axis',(1.,0.,0.));
#14283=DIRECTION('center_axis',(-0.707106781186539,0.,0.707106781186556));
#14284=DIRECTION('ref_axis',(-0.707106781186556,0.,-0.707106781186539));
#14285=DIRECTION('center_axis',(0.,1.,0.));
#14286=DIRECTION('ref_axis',(1.,0.,0.));
#14287=DIRECTION('center_axis',(-1.,-1.11022302462516E-14,0.));
#14288=DIRECTION('ref_axis',(-1.11022302462516E-14,1.,0.));
#14289=DIRECTION('center_axis',(0.,1.,0.));
#14290=DIRECTION('ref_axis',(0.,0.,-1.));
#14291=DIRECTION('center_axis',(0.,0.,-1.));
#14292=DIRECTION('ref_axis',(1.,3.33066907387547E-14,0.));
#14293=DIRECTION('center_axis',(-0.707106781186548,0.,0.707106781186548));
#14294=DIRECTION('ref_axis',(0.707106781186548,0.,0.707106781186548));
#14295=DIRECTION('center_axis',(-0.707106781186545,1.96261557335471E-14,
0.70710678118655));
#14296=DIRECTION('ref_axis',(0.70710678118655,-4.24411161318039E-31,0.707106781186545));
#14297=DIRECTION('center_axis',(0.,-1.,0.));
#14298=DIRECTION('ref_axis',(0.,0.,-1.));
#14299=DIRECTION('center_axis',(0.,1.,0.));
#14300=DIRECTION('ref_axis',(0.,0.,1.));
#14301=DIRECTION('center_axis',(-1.,0.,0.));
#14302=DIRECTION('ref_axis',(0.,0.,1.));
#14303=DIRECTION('center_axis',(0.,0.,-1.));
#14304=DIRECTION('ref_axis',(-1.,0.,0.));
#14305=DIRECTION('center_axis',(0.,0.,-1.));
#14306=DIRECTION('ref_axis',(-1.,0.,0.));
#14307=DIRECTION('center_axis',(0.,1.,0.));
#14308=DIRECTION('ref_axis',(1.,0.,0.));
#14309=DIRECTION('center_axis',(-1.,5.55111512312578E-15,0.));
#14310=DIRECTION('ref_axis',(5.55111512312578E-15,1.,0.));
#14311=DIRECTION('center_axis',(-0.710144927536232,-0.704055524724123,3.94209624685744E-15));
#14312=DIRECTION('ref_axis',(-0.704055524724123,0.710144927536232,2.77555756156289E-15));
#14313=DIRECTION('center_axis',(0.,1.,0.));
#14314=DIRECTION('ref_axis',(1.,0.,0.));
#14315=DIRECTION('center_axis',(-1.,0.,-2.22044604925031E-14));
#14316=DIRECTION('ref_axis',(2.22044604925031E-14,0.,-1.));
#14317=DIRECTION('center_axis',(-0.797101449275362,-0.603845410318832,0.));
#14318=DIRECTION('ref_axis',(-0.603845410318832,0.797101449275361,0.));
#14319=DIRECTION('center_axis',(0.,0.,1.));
#14320=DIRECTION('ref_axis',(1.,0.,0.));
#14321=DIRECTION('center_axis',(-0.518508516521693,-0.855072463768114,0.));
#14322=DIRECTION('ref_axis',(0.855072463768114,-0.518508516521693,0.));
#14323=DIRECTION('center_axis',(0.,-1.,0.));
#14324=DIRECTION('ref_axis',(0.,0.,-1.));
#14325=DIRECTION('center_axis',(0.,-1.,0.));
#14326=DIRECTION('ref_axis',(0.,0.,1.));
#14327=DIRECTION('center_axis',(1.,0.,0.));
#14328=DIRECTION('ref_axis',(0.,0.,-1.));
#14329=DIRECTION('center_axis',(-1.,0.,0.));
#14330=DIRECTION('ref_axis',(0.,0.,1.));
#14331=DIRECTION('center_axis',(1.,0.,0.));
#14332=DIRECTION('ref_axis',(0.,0.,-1.));
#14333=DIRECTION('center_axis',(0.,0.,1.));
#14334=DIRECTION('ref_axis',(1.,0.,0.));
#14335=DIRECTION('center_axis',(-0.739130434782608,-0.673562321079551,0.));
#14336=DIRECTION('ref_axis',(0.673562321079551,-0.739130434782608,0.));
#14337=DIRECTION('center_axis',(0.,0.,-1.));
#14338=DIRECTION('ref_axis',(1.,0.,0.));
#14339=DIRECTION('center_axis',(0.,1.,0.));
#14340=DIRECTION('ref_axis',(0.,0.,1.));
#14341=DIRECTION('center_axis',(0.,0.,-1.));
#14342=DIRECTION('ref_axis',(1.,0.,0.));
#14343=DIRECTION('center_axis',(0.,0.,-1.));
#14344=DIRECTION('ref_axis',(-1.,0.,0.));
#14345=DIRECTION('center_axis',(0.,0.,-1.));
#14346=DIRECTION('ref_axis',(-1.,0.,0.));
#14347=DIRECTION('center_axis',(0.,1.,0.));
#14348=DIRECTION('ref_axis',(0.,0.,1.));
#14349=DIRECTION('center_axis',(0.,-1.,0.));
#14350=DIRECTION('ref_axis',(0.,0.,1.));
#14351=DIRECTION('center_axis',(0.,0.,1.));
#14352=DIRECTION('ref_axis',(1.,0.,0.));
#14353=DIRECTION('center_axis',(0.,0.,-1.));
#14354=DIRECTION('ref_axis',(-1.,0.,0.));
#14355=DIRECTION('center_axis',(1.,0.,0.));
#14356=DIRECTION('ref_axis',(0.,0.,-1.));
#14357=DIRECTION('center_axis',(1.,0.,5.55111512312578E-15));
#14358=DIRECTION('ref_axis',(5.55111512312578E-15,0.,-1.));
#14359=DIRECTION('center_axis',(-1.,0.,0.));
#14360=DIRECTION('ref_axis',(0.,0.,1.));
#14361=DIRECTION('center_axis',(0.518508516521693,0.855072463768114,1.00999525007457E-15));
#14362=DIRECTION('ref_axis',(0.855072463768114,-0.518508516521693,-8.14669008397628E-32));
#14363=DIRECTION('center_axis',(0.,1.,0.));
#14364=DIRECTION('ref_axis',(0.,0.,1.));
#14365=DIRECTION('center_axis',(1.,0.,0.));
#14366=DIRECTION('ref_axis',(0.,0.,1.));
#14367=DIRECTION('center_axis',(0.,1.,0.));
#14368=DIRECTION('ref_axis',(0.,0.,1.));
#14369=DIRECTION('center_axis',(0.,0.,1.));
#14370=DIRECTION('ref_axis',(-1.,0.,0.));
#14371=DIRECTION('center_axis',(0.,1.,0.));
#14372=DIRECTION('ref_axis',(0.,0.,1.));
#14373=DIRECTION('center_axis',(0.,1.,0.));
#14374=DIRECTION('ref_axis',(1.,0.,0.));
#14375=DIRECTION('center_axis',(-0.710144927536229,-0.704055524724125,0.));
#14376=DIRECTION('ref_axis',(-0.704055524724125,0.710144927536229,0.));
#14377=DIRECTION('center_axis',(0.,0.,1.));
#14378=DIRECTION('ref_axis',(1.,0.,0.));
#14379=DIRECTION('center_axis',(0.710144927536229,0.704055524724125,0.));
#14380=DIRECTION('ref_axis',(-0.704055524724125,0.710144927536229,0.));
#14381=DIRECTION('center_axis',(-1.,0.,0.));
#14382=DIRECTION('ref_axis',(0.,0.,1.));
#14383=DIRECTION('center_axis',(1.,0.,5.55111512312578E-15));
#14384=DIRECTION('ref_axis',(5.55111512312578E-15,0.,-1.));
#14385=DIRECTION('center_axis',(0.,0.,1.));
#14386=DIRECTION('ref_axis',(1.,0.,0.));
#14387=DIRECTION('center_axis',(0.,0.,1.));
#14388=DIRECTION('ref_axis',(1.,0.,0.));
#14389=DIRECTION('center_axis',(0.,1.,0.));
#14390=DIRECTION('ref_axis',(0.,0.,1.));
#14391=DIRECTION('center_axis',(0.,0.,-1.));
#14392=DIRECTION('ref_axis',(-1.,0.,0.));
#14393=DIRECTION('center_axis',(-0.518508516521689,-0.855072463768117,4.74660568499161E-15));
#14394=DIRECTION('ref_axis',(0.855072463768117,-0.518508516521689,-1.27467223778887E-31));
#14395=DIRECTION('center_axis',(0.,1.,0.));
#14396=DIRECTION('ref_axis',(1.,0.,0.));
#14397=DIRECTION('center_axis',(0.,1.,0.));
#14398=DIRECTION('ref_axis',(0.,0.,1.));
#14399=DIRECTION('center_axis',(1.,0.,0.));
#14400=DIRECTION('ref_axis',(0.,0.,1.));
#14401=DIRECTION('center_axis',(0.,1.,0.));
#14402=DIRECTION('ref_axis',(0.,0.,1.));
#14403=DIRECTION('center_axis',(0.,0.,1.));
#14404=DIRECTION('ref_axis',(-1.,0.,0.));
#14405=DIRECTION('center_axis',(-1.,0.,0.));
#14406=DIRECTION('ref_axis',(0.,0.,1.));
#14407=DIRECTION('center_axis',(1.,-5.55111512312578E-15,0.));
#14408=DIRECTION('ref_axis',(5.55111512312578E-15,1.,0.));
#14409=DIRECTION('center_axis',(0.,-1.,0.));
#14410=DIRECTION('ref_axis',(0.,0.,-1.));
#14411=DIRECTION('center_axis',(0.,0.,-1.));
#14412=DIRECTION('ref_axis',(-1.,0.,0.));
#14413=DIRECTION('center_axis',(0.,0.,1.));
#14414=DIRECTION('ref_axis',(1.,0.,0.));
#14415=DIRECTION('center_axis',(0.,1.,0.));
#14416=DIRECTION('ref_axis',(1.,0.,0.));
#14417=DIRECTION('center_axis',(-0.710144927536232,-0.704055524724123,3.94209624685744E-15));
#14418=DIRECTION('ref_axis',(-0.704055524724123,0.710144927536232,2.77555756156289E-15));
#14419=DIRECTION('center_axis',(0.518508516521693,0.855072463768114,0.));
#14420=DIRECTION('ref_axis',(0.855072463768114,-0.518508516521693,0.));
#14421=DIRECTION('center_axis',(0.,0.,-1.));
#14422=DIRECTION('ref_axis',(-1.,0.,0.));
#14423=DIRECTION('axis',(0.,0.,1.));
#14424=DIRECTION('refdir',(1.,0.,0.));
#14425=DIRECTION('center_axis',(0.,0.,1.));
#14426=DIRECTION('ref_axis',(1.,0.,0.));
#14427=DIRECTION('center_axis',(0.,0.,1.));
#14428=DIRECTION('ref_axis',(1.,0.,0.));
#14429=DIRECTION('',(0.707106781186541,8.65956056235485E-17,-0.707106781186554));
#14430=DIRECTION('center_axis',(0.,0.,-1.));
#14431=DIRECTION('ref_axis',(1.,0.,0.));
#14432=DIRECTION('center_axis',(0.,0.,-1.));
#14433=DIRECTION('ref_axis',(1.,0.,0.));
#14434=DIRECTION('center_axis',(0.,0.,1.));
#14435=DIRECTION('ref_axis',(1.,0.,0.));
#14436=DIRECTION('center_axis',(0.,0.,1.));
#14437=DIRECTION('ref_axis',(1.,0.,0.));
#14438=DIRECTION('center_axis',(0.,0.,1.));
#14439=DIRECTION('ref_axis',(1.,0.,0.));
#14440=DIRECTION('',(0.707106781186529,8.65956056235471E-17,-0.707106781186566));
#14441=DIRECTION('center_axis',(0.,0.,-1.));
#14442=DIRECTION('ref_axis',(1.,0.,0.));
#14443=DIRECTION('center_axis',(0.,0.,1.));
#14444=DIRECTION('ref_axis',(1.,0.,0.));
#14445=DIRECTION('center_axis',(0.,0.,1.));
#14446=DIRECTION('ref_axis',(1.,0.,0.));
#14447=DIRECTION('center_axis',(0.,0.,1.));
#14448=DIRECTION('ref_axis',(1.,0.,0.));
#14449=DIRECTION('',(0.707106781186545,8.6595605623549E-17,-0.70710678118655));
#14450=DIRECTION('center_axis',(0.,0.,-1.));
#14451=DIRECTION('ref_axis',(1.,0.,0.));
#14452=DIRECTION('center_axis',(0.,0.,-1.));
#14453=DIRECTION('ref_axis',(1.83697019872103E-16,-1.,0.));
#14454=DIRECTION('center_axis',(0.,0.,1.));
#14455=DIRECTION('ref_axis',(1.,0.,0.));
#14456=DIRECTION('',(0.,0.,-1.));
#14457=DIRECTION('center_axis',(0.,0.,-1.));
#14458=DIRECTION('ref_axis',(-1.,0.,0.));
#14459=DIRECTION('',(0.,0.,-1.));
#14460=DIRECTION('center_axis',(0.,0.,-1.));
#14461=DIRECTION('ref_axis',(-1.,0.,0.));
#14462=DIRECTION('center_axis',(0.,0.,1.));
#14463=DIRECTION('ref_axis',(1.,0.,0.));
#14464=DIRECTION('',(0.,0.,-1.));
#14465=DIRECTION('center_axis',(0.,0.,1.));
#14466=DIRECTION('ref_axis',(1.,0.,0.));
#14467=DIRECTION('center_axis',(0.,0.,1.));
#14468=DIRECTION('ref_axis',(1.,0.,0.));
#14469=DIRECTION('center_axis',(0.,0.,1.));
#14470=DIRECTION('ref_axis',(1.,0.,0.));
#14471=DIRECTION('center_axis',(0.,0.,1.));
#14472=DIRECTION('ref_axis',(1.,0.,0.));
#14473=DIRECTION('center_axis',(0.,0.,1.));
#14474=DIRECTION('ref_axis',(1.,0.,0.));
#14475=DIRECTION('center_axis',(0.,0.,1.));
#14476=DIRECTION('ref_axis',(1.,0.,0.));
#14477=DIRECTION('center_axis',(0.,0.,1.));
#14478=DIRECTION('ref_axis',(1.,0.,0.));
#14479=DIRECTION('center_axis',(0.,0.,1.));
#14480=DIRECTION('ref_axis',(1.,0.,0.));
#14481=DIRECTION('center_axis',(0.,0.,1.));
#14482=DIRECTION('ref_axis',(1.,0.,0.));
#14483=DIRECTION('center_axis',(0.,0.,1.));
#14484=DIRECTION('ref_axis',(1.,0.,0.));
#14485=DIRECTION('center_axis',(0.,0.,1.));
#14486=DIRECTION('ref_axis',(1.,0.,0.));
#14487=DIRECTION('center_axis',(0.,0.,1.));
#14488=DIRECTION('ref_axis',(1.,0.,0.));
#14489=DIRECTION('center_axis',(0.,0.,1.));
#14490=DIRECTION('ref_axis',(1.,0.,0.));
#14491=DIRECTION('center_axis',(0.,0.,1.));
#14492=DIRECTION('ref_axis',(1.,0.,0.));
#14493=DIRECTION('center_axis',(0.,0.,1.));
#14494=DIRECTION('ref_axis',(1.,0.,0.));
#14495=DIRECTION('center_axis',(0.,0.,1.));
#14496=DIRECTION('ref_axis',(1.,0.,0.));
#14497=DIRECTION('center_axis',(0.,0.,1.));
#14498=DIRECTION('ref_axis',(1.,0.,0.));
#14499=DIRECTION('center_axis',(0.,0.,-1.));
#14500=DIRECTION('ref_axis',(1.,-3.5527136788005E-14,0.));
#14501=DIRECTION('center_axis',(0.,0.,1.));
#14502=DIRECTION('ref_axis',(1.,0.,0.));
#14503=DIRECTION('center_axis',(0.,0.,1.));
#14504=DIRECTION('ref_axis',(1.,0.,0.));
#14505=DIRECTION('center_axis',(0.,0.,1.));
#14506=DIRECTION('ref_axis',(1.,0.,0.));
#14507=DIRECTION('center_axis',(0.,0.,-1.));
#14508=DIRECTION('ref_axis',(-1.,0.,0.));
#14509=DIRECTION('center_axis',(0.,0.,1.));
#14510=DIRECTION('ref_axis',(1.,0.,0.));
#14511=DIRECTION('',(0.,0.,1.));
#14512=DIRECTION('center_axis',(0.,0.,1.));
#14513=DIRECTION('ref_axis',(1.,0.,0.));
#14514=DIRECTION('',(0.,0.,-1.));
#14515=DIRECTION('center_axis',(0.,0.,1.));
#14516=DIRECTION('ref_axis',(1.,0.,0.));
#14517=DIRECTION('',(0.,0.,1.));
#14518=DIRECTION('center_axis',(0.,0.,1.));
#14519=DIRECTION('ref_axis',(1.,0.,0.));
#14520=DIRECTION('center_axis',(0.,0.,1.));
#14521=DIRECTION('ref_axis',(1.,0.,0.));
#14522=DIRECTION('',(0.,0.,-1.));
#14523=DIRECTION('center_axis',(0.,0.,1.));
#14524=DIRECTION('ref_axis',(1.,0.,0.));
#14525=DIRECTION('center_axis',(0.,0.,1.));
#14526=DIRECTION('ref_axis',(1.,0.,0.));
#14527=DIRECTION('',(0.,0.,-1.));
#14528=DIRECTION('center_axis',(0.,0.,1.));
#14529=DIRECTION('ref_axis',(1.,0.,0.));
#14530=DIRECTION('',(0.,0.,-1.));
#14531=DIRECTION('',(0.,0.,-1.));
#14532=DIRECTION('center_axis',(0.,0.,1.));
#14533=DIRECTION('ref_axis',(1.,0.,0.));
#14534=DIRECTION('',(0.,0.,-1.));
#14535=DIRECTION('center_axis',(0.,0.,1.));
#14536=DIRECTION('ref_axis',(1.,0.,0.));
#14537=DIRECTION('',(0.,0.,-1.));
#14538=DIRECTION('center_axis',(0.,0.,1.));
#14539=DIRECTION('ref_axis',(1.,0.,0.));
#14540=DIRECTION('',(0.,0.,-1.));
#14541=DIRECTION('center_axis',(0.,0.,1.));
#14542=DIRECTION('ref_axis',(1.,0.,0.));
#14543=DIRECTION('',(0.,0.,-1.));
#14544=DIRECTION('center_axis',(0.,0.,1.));
#14545=DIRECTION('ref_axis',(1.,0.,0.));
#14546=DIRECTION('',(0.,0.,-1.));
#14547=DIRECTION('center_axis',(0.,0.,1.));
#14548=DIRECTION('ref_axis',(1.,0.,0.));
#14549=DIRECTION('',(0.,0.,-1.));
#14550=DIRECTION('center_axis',(0.,0.,1.));
#14551=DIRECTION('ref_axis',(1.,0.,0.));
#14552=DIRECTION('',(0.,0.,-1.));
#14553=DIRECTION('center_axis',(0.,0.,1.));
#14554=DIRECTION('ref_axis',(1.,0.,0.));
#14555=DIRECTION('center_axis',(0.,0.,1.));
#14556=DIRECTION('ref_axis',(1.,0.,0.));
#14557=DIRECTION('',(0.,0.,-1.));
#14558=DIRECTION('center_axis',(0.,0.,1.));
#14559=DIRECTION('ref_axis',(1.,0.,0.));
#14560=DIRECTION('',(0.,0.,-1.));
#14561=DIRECTION('',(0.,0.,-1.));
#14562=DIRECTION('center_axis',(0.,0.,1.));
#14563=DIRECTION('ref_axis',(1.,0.,0.));
#14564=DIRECTION('',(0.,0.,-1.));
#14565=DIRECTION('center_axis',(0.,0.,1.));
#14566=DIRECTION('ref_axis',(1.,0.,0.));
#14567=DIRECTION('',(0.,0.,-1.));
#14568=DIRECTION('center_axis',(0.,0.,1.));
#14569=DIRECTION('ref_axis',(1.,0.,0.));
#14570=DIRECTION('',(0.,0.,-1.));
#14571=DIRECTION('center_axis',(0.,0.,1.));
#14572=DIRECTION('ref_axis',(1.,0.,0.));
#14573=DIRECTION('',(0.,0.,-1.));
#14574=DIRECTION('center_axis',(0.,0.,1.));
#14575=DIRECTION('ref_axis',(1.,0.,0.));
#14576=DIRECTION('',(0.,0.,-1.));
#14577=DIRECTION('center_axis',(0.,0.,1.));
#14578=DIRECTION('ref_axis',(1.,0.,0.));
#14579=DIRECTION('center_axis',(0.,0.,-1.));
#14580=DIRECTION('ref_axis',(-1.,0.,0.));
#14581=DIRECTION('',(0.,0.,1.));
#14582=DIRECTION('center_axis',(0.,0.,-1.));
#14583=DIRECTION('ref_axis',(-1.,0.,0.));
#14584=DIRECTION('',(0.,0.,1.));
#14585=DIRECTION('center_axis',(0.,0.,1.));
#14586=DIRECTION('ref_axis',(1.,0.,0.));
#14587=DIRECTION('center_axis',(0.,0.,1.));
#14588=DIRECTION('ref_axis',(1.,0.,0.));
#14589=DIRECTION('',(0.,-1.,0.));
#14590=DIRECTION('',(1.,0.,0.));
#14591=DIRECTION('',(0.,1.,0.));
#14592=DIRECTION('center_axis',(0.,0.,1.));
#14593=DIRECTION('ref_axis',(0.809016994374947,0.587785252292474,0.));
#14594=DIRECTION('',(0.587785252292474,-0.809016994374947,0.));
#14595=DIRECTION('',(0.809016994374947,0.587785252292474,0.));
#14596=DIRECTION('',(-0.587785252292474,0.809016994374947,0.));
#14597=DIRECTION('center_axis',(0.,0.,1.));
#14598=DIRECTION('ref_axis',(0.309016994374945,0.951056516295155,0.));
#14599=DIRECTION('',(0.951056516295154,-0.309016994374945,0.));
#14600=DIRECTION('',(0.309016994374945,0.951056516295154,0.));
#14601=DIRECTION('',(-0.951056516295154,0.309016994374945,0.));
#14602=DIRECTION('center_axis',(0.,0.,1.));
#14603=DIRECTION('ref_axis',(-0.309016994374952,0.951056516295152,0.));
#14604=DIRECTION('',(0.951056516295152,0.309016994374952,0.));
#14605=DIRECTION('',(-0.309016994374952,0.951056516295152,0.));
#14606=DIRECTION('',(-0.951056516295152,-0.309016994374952,0.));
#14607=DIRECTION('center_axis',(0.,0.,1.));
#14608=DIRECTION('ref_axis',(-0.809016994374951,0.587785252292469,0.));
#14609=DIRECTION('',(0.587785252292469,0.809016994374951,0.));
#14610=DIRECTION('',(-0.809016994374951,0.587785252292468,0.));
#14611=DIRECTION('',(-0.587785252292468,-0.809016994374951,0.));
#14612=DIRECTION('center_axis',(0.,0.,1.));
#14613=DIRECTION('ref_axis',(-1.,0.,0.));
#14614=DIRECTION('',(0.,1.,0.));
#14615=DIRECTION('',(-1.,0.,0.));
#14616=DIRECTION('',(0.,-1.,0.));
#14617=DIRECTION('center_axis',(0.,0.,1.));
#14618=DIRECTION('ref_axis',(-0.809016994374942,-0.58778525229248,0.));
#14619=DIRECTION('',(-0.58778525229248,0.809016994374942,0.));
#14620=DIRECTION('',(-0.809016994374942,-0.58778525229248,0.));
#14621=DIRECTION('',(0.58778525229248,-0.809016994374942,0.));
#14622=DIRECTION('center_axis',(0.,0.,1.));
#14623=DIRECTION('ref_axis',(-0.309016994374938,-0.951056516295157,0.));
#14624=DIRECTION('',(-0.951056516295157,0.309016994374938,0.));
#14625=DIRECTION('',(-0.309016994374938,-0.951056516295157,0.));
#14626=DIRECTION('',(0.951056516295157,-0.309016994374938,0.));
#14627=DIRECTION('center_axis',(0.,0.,1.));
#14628=DIRECTION('ref_axis',(0.309016994374958,-0.95105651629515,0.));
#14629=DIRECTION('',(-0.95105651629515,-0.309016994374958,0.));
#14630=DIRECTION('',(0.309016994374958,-0.95105651629515,0.));
#14631=DIRECTION('',(0.95105651629515,0.309016994374958,0.));
#14632=DIRECTION('center_axis',(0.,0.,1.));
#14633=DIRECTION('ref_axis',(0.809016994374955,-0.587785252292463,0.));
#14634=DIRECTION('',(-0.587785252292463,-0.809016994374955,0.));
#14635=DIRECTION('',(0.809016994374955,-0.587785252292463,0.));
#14636=DIRECTION('',(0.587785252292462,0.809016994374955,0.));
#14637=DIRECTION('center_axis',(0.,0.,1.));
#14638=DIRECTION('ref_axis',(1.,0.,0.));
#14639=DIRECTION('',(0.777145961456963,0.629320391049847,0.));
#14640=DIRECTION('center_axis',(0.,0.,-1.));
#14641=DIRECTION('ref_axis',(0.809016994374955,-0.587785252292462,0.));
#14642=DIRECTION('',(0.587785252292462,0.809016994374955,0.));
#14643=DIRECTION('',(0.809016994374955,-0.587785252292463,0.));
#14644=DIRECTION('',(-0.587785252292463,-0.809016994374955,0.));
#14645=DIRECTION('',(0.258819045102522,0.965925826289068,0.));
#14646=DIRECTION('center_axis',(0.,0.,-1.));
#14647=DIRECTION('ref_axis',(1.,0.,0.));
#14648=DIRECTION('',(0.,1.,0.));
#14649=DIRECTION('',(1.,0.,0.));
#14650=DIRECTION('',(0.,-1.,0.));
#14651=DIRECTION('',(-0.3583679495453,0.933580426497202,0.));
#14652=DIRECTION('center_axis',(0.,0.,-1.));
#14653=DIRECTION('ref_axis',(0.809016994374947,0.587785252292474,0.));
#14654=DIRECTION('',(-0.587785252292474,0.809016994374947,0.));
#14655=DIRECTION('',(0.809016994374947,0.587785252292474,0.));
#14656=DIRECTION('',(0.587785252292474,-0.809016994374947,0.));
#14657=DIRECTION('',(-0.838670567945425,0.544639035015026,0.));
#14658=DIRECTION('center_axis',(0.,0.,-1.));
#14659=DIRECTION('ref_axis',(0.309016994374945,0.951056516295154,0.));
#14660=DIRECTION('',(-0.951056516295154,0.309016994374945,0.));
#14661=DIRECTION('',(0.309016994374945,0.951056516295155,0.));
#14662=DIRECTION('',(0.951056516295154,-0.309016994374945,0.));
#14663=DIRECTION('',(-0.998629534754574,-0.0523359562429468,0.));
#14664=DIRECTION('center_axis',(0.,0.,-1.));
#14665=DIRECTION('ref_axis',(-0.309016994374952,0.951056516295152,0.));
#14666=DIRECTION('',(-0.951056516295152,-0.309016994374952,0.));
#14667=DIRECTION('',(-0.309016994374952,0.951056516295152,0.));
#14668=DIRECTION('',(0.951056516295152,0.309016994374952,0.));
#14669=DIRECTION('',(-0.777145961456968,-0.629320391049841,0.));
#14670=DIRECTION('center_axis',(0.,0.,-1.));
#14671=DIRECTION('ref_axis',(-0.809016994374951,0.587785252292469,0.));
#14672=DIRECTION('',(-0.587785252292468,-0.809016994374951,0.));
#14673=DIRECTION('',(-0.809016994374951,0.587785252292469,0.));
#14674=DIRECTION('',(0.587785252292469,0.809016994374951,0.));
#14675=DIRECTION('',(-0.258819045102522,-0.965925826289068,0.));
#14676=DIRECTION('center_axis',(0.,0.,-1.));
#14677=DIRECTION('ref_axis',(-1.,0.,0.));
#14678=DIRECTION('',(0.,-1.,0.));
#14679=DIRECTION('',(-1.,0.,0.));
#14680=DIRECTION('',(0.,1.,0.));
#14681=DIRECTION('',(0.358367949545307,-0.933580426497199,0.));
#14682=DIRECTION('center_axis',(0.,0.,-1.));
#14683=DIRECTION('ref_axis',(-0.809016994374942,-0.58778525229248,0.));
#14684=DIRECTION('',(0.58778525229248,-0.809016994374942,0.));
#14685=DIRECTION('',(-0.809016994374942,-0.58778525229248,0.));
#14686=DIRECTION('',(-0.58778525229248,0.809016994374942,0.));
#14687=DIRECTION('',(0.838670567945429,-0.54463903501502,0.));
#14688=DIRECTION('center_axis',(0.,0.,-1.));
#14689=DIRECTION('ref_axis',(-0.309016994374938,-0.951056516295157,0.));
#14690=DIRECTION('',(0.951056516295157,-0.309016994374938,0.));
#14691=DIRECTION('',(-0.309016994374938,-0.951056516295157,0.));
#14692=DIRECTION('',(-0.951056516295157,0.309016994374938,0.));
#14693=DIRECTION('',(0.998629534754573,0.0523359562429538,0.));
#14694=DIRECTION('center_axis',(0.,0.,-1.));
#14695=DIRECTION('ref_axis',(0.309016994374958,-0.95105651629515,0.));
#14696=DIRECTION('',(0.95105651629515,0.309016994374958,0.));
#14697=DIRECTION('',(0.309016994374958,-0.95105651629515,0.));
#14698=DIRECTION('',(-0.95105651629515,-0.309016994374958,0.));
#14699=DIRECTION('',(2.6394692217289E-16,1.,0.));
#14700=DIRECTION('',(2.6394692217289E-16,-1.,0.));
#14701=DIRECTION('',(-1.,0.,0.));
#14702=DIRECTION('center_axis',(0.,0.,1.));
#14703=DIRECTION('ref_axis',(1.,0.,0.));
#14704=DIRECTION('',(-2.6394692217289E-16,-1.,0.));
#14705=DIRECTION('',(1.,0.,0.));
#14706=DIRECTION('',(-2.6394692217289E-16,1.,0.));
#14707=DIRECTION('center_axis',(0.,0.,1.));
#14708=DIRECTION('ref_axis',(1.,0.,0.));
#14709=DIRECTION('center_axis',(0.,0.,1.));
#14710=DIRECTION('ref_axis',(1.,0.,0.));
#14711=DIRECTION('center_axis',(0.,1.,0.));
#14712=DIRECTION('ref_axis',(0.,0.,1.));
#14713=DIRECTION('',(0.,0.,-1.));
#14714=DIRECTION('',(-1.,0.,0.));
#14715=DIRECTION('',(0.,0.,-1.));
#14716=DIRECTION('center_axis',(-1.,0.,0.));
#14717=DIRECTION('ref_axis',(0.,0.,1.));
#14718=DIRECTION('center_axis',(1.,0.,0.));
#14719=DIRECTION('ref_axis',(0.,0.,1.));
#14720=DIRECTION('',(0.,0.,-1.));
#14721=DIRECTION('',(0.,1.,0.));
#14722=DIRECTION('center_axis',(0.,0.,-1.));
#14723=DIRECTION('ref_axis',(-1.,0.,0.));
#14724=DIRECTION('',(0.,0.,-1.));
#14725=DIRECTION('center_axis',(0.,0.,-1.));
#14726=DIRECTION('ref_axis',(1.,0.,0.));
#14727=DIRECTION('center_axis',(-0.965925826289068,0.258819045102522,0.));
#14728=DIRECTION('ref_axis',(-0.258819045102522,-0.965925826289068,0.));
#14729=DIRECTION('',(0.258819045102522,0.965925826289068,0.));
#14730=DIRECTION('center_axis',(1.,0.,0.));
#14731=DIRECTION('ref_axis',(0.,0.,-1.));
#14732=DIRECTION('center_axis',(-1.,0.,0.));
#14733=DIRECTION('ref_axis',(0.,0.,-1.));
#14734=DIRECTION('',(0.,-1.,0.));
#14735=DIRECTION('center_axis',(-1.,0.,0.));
#14736=DIRECTION('ref_axis',(0.,0.,1.));
#14737=DIRECTION('center_axis',(-0.587785252292474,0.809016994374947,0.));
#14738=DIRECTION('ref_axis',(-0.809016994374947,-0.587785252292474,0.));
#14739=DIRECTION('',(0.,0.,-1.));
#14740=DIRECTION('',(-0.809016994374947,-0.587785252292474,0.));
#14741=DIRECTION('',(0.,0.,-1.));
#14742=DIRECTION('center_axis',(-0.809016994374947,-0.587785252292474,0.));
#14743=DIRECTION('ref_axis',(0.587785252292474,-0.809016994374947,0.));
#14744=DIRECTION('center_axis',(0.809016994374947,0.587785252292474,0.));
#14745=DIRECTION('ref_axis',(0.587785252292474,-0.809016994374947,0.));
#14746=DIRECTION('',(0.,0.,-1.));
#14747=DIRECTION('',(-0.587785252292474,0.809016994374947,0.));
#14748=DIRECTION('center_axis',(0.,0.,-1.));
#14749=DIRECTION('ref_axis',(-1.,0.,0.));
#14750=DIRECTION('',(0.,0.,-1.));
#14751=DIRECTION('center_axis',(0.,0.,-1.));
#14752=DIRECTION('ref_axis',(0.809016994374947,0.587785252292474,0.));
#14753=DIRECTION('center_axis',(-0.933580426497202,-0.3583679495453,0.));
#14754=DIRECTION('ref_axis',(0.3583679495453,-0.933580426497202,0.));
#14755=DIRECTION('',(-0.3583679495453,0.933580426497202,0.));
#14756=DIRECTION('center_axis',(0.809016994374947,0.587785252292474,0.));
#14757=DIRECTION('ref_axis',(-0.587785252292474,0.809016994374947,0.));
#14758=DIRECTION('center_axis',(-0.809016994374947,-0.587785252292474,0.));
#14759=DIRECTION('ref_axis',(-0.587785252292474,0.809016994374947,0.));
#14760=DIRECTION('',(0.587785252292474,-0.809016994374947,0.));
#14761=DIRECTION('center_axis',(-0.951056516295155,0.309016994374945,0.));
#14762=DIRECTION('ref_axis',(-0.309016994374945,-0.951056516295155,0.));
#14763=DIRECTION('',(0.,0.,-1.));
#14764=DIRECTION('',(-0.309016994374945,-0.951056516295154,0.));
#14765=DIRECTION('',(0.,0.,-1.));
#14766=DIRECTION('center_axis',(-0.309016994374945,-0.951056516295155,0.));
#14767=DIRECTION('ref_axis',(0.951056516295155,-0.309016994374945,0.));
#14768=DIRECTION('center_axis',(0.309016994374945,0.951056516295155,0.));
#14769=DIRECTION('ref_axis',(0.951056516295154,-0.309016994374945,0.));
#14770=DIRECTION('',(0.,0.,-1.));
#14771=DIRECTION('',(-0.951056516295155,0.309016994374945,0.));
#14772=DIRECTION('center_axis',(0.,0.,-1.));
#14773=DIRECTION('ref_axis',(-1.,0.,0.));
#14774=DIRECTION('',(0.,0.,-1.));
#14775=DIRECTION('center_axis',(0.,0.,-1.));
#14776=DIRECTION('ref_axis',(0.309016994374945,0.951056516295154,0.));
#14777=DIRECTION('center_axis',(-0.544639035015026,-0.838670567945425,0.));
#14778=DIRECTION('ref_axis',(0.838670567945425,-0.544639035015026,0.));
#14779=DIRECTION('',(-0.838670567945425,0.544639035015026,0.));
#14780=DIRECTION('center_axis',(0.309016994374945,0.951056516295155,0.));
#14781=DIRECTION('ref_axis',(-0.951056516295155,0.309016994374945,0.));
#14782=DIRECTION('center_axis',(-0.309016994374945,-0.951056516295155,0.));
#14783=DIRECTION('ref_axis',(-0.951056516295154,0.309016994374945,0.));
#14784=DIRECTION('',(0.951056516295154,-0.309016994374945,0.));
#14785=DIRECTION('center_axis',(-0.951056516295152,-0.309016994374952,0.));
#14786=DIRECTION('ref_axis',(0.309016994374952,-0.951056516295152,0.));
#14787=DIRECTION('',(0.,0.,-1.));
#14788=DIRECTION('',(0.309016994374952,-0.951056516295152,0.));
#14789=DIRECTION('',(0.,0.,-1.));
#14790=DIRECTION('center_axis',(0.309016994374952,-0.951056516295152,0.));
#14791=DIRECTION('ref_axis',(0.951056516295152,0.309016994374952,0.));
#14792=DIRECTION('center_axis',(-0.309016994374952,0.951056516295152,0.));
#14793=DIRECTION('ref_axis',(0.951056516295152,0.309016994374952,0.));
#14794=DIRECTION('',(0.,0.,-1.));
#14795=DIRECTION('',(-0.951056516295152,-0.309016994374952,0.));
#14796=DIRECTION('center_axis',(0.,0.,-1.));
#14797=DIRECTION('ref_axis',(-1.,0.,0.));
#14798=DIRECTION('',(0.,0.,-1.));
#14799=DIRECTION('center_axis',(0.,0.,-1.));
#14800=DIRECTION('ref_axis',(-0.309016994374952,0.951056516295152,0.));
#14801=DIRECTION('center_axis',(0.0523359562429468,-0.998629534754574,0.));
#14802=DIRECTION('ref_axis',(0.998629534754574,0.0523359562429469,0.));
#14803=DIRECTION('',(-0.998629534754574,-0.0523359562429468,0.));
#14804=DIRECTION('center_axis',(-0.309016994374952,0.951056516295152,0.));
#14805=DIRECTION('ref_axis',(-0.951056516295152,-0.309016994374952,0.));
#14806=DIRECTION('center_axis',(0.309016994374952,-0.951056516295152,0.));
#14807=DIRECTION('ref_axis',(-0.951056516295152,-0.309016994374952,0.));
#14808=DIRECTION('',(0.951056516295152,0.309016994374952,0.));
#14809=DIRECTION('center_axis',(-0.587785252292469,-0.809016994374951,0.));
#14810=DIRECTION('ref_axis',(0.809016994374951,-0.587785252292469,0.));
#14811=DIRECTION('',(0.,0.,-1.));
#14812=DIRECTION('',(0.809016994374951,-0.587785252292468,0.));
#14813=DIRECTION('',(0.,0.,-1.));
#14814=DIRECTION('center_axis',(0.809016994374951,-0.587785252292469,0.));
#14815=DIRECTION('ref_axis',(0.587785252292469,0.809016994374951,0.));
#14816=DIRECTION('center_axis',(-0.809016994374951,0.587785252292469,0.));
#14817=DIRECTION('ref_axis',(0.587785252292469,0.809016994374951,0.));
#14818=DIRECTION('',(0.,0.,-1.));
#14819=DIRECTION('',(-0.587785252292469,-0.809016994374951,0.));
#14820=DIRECTION('center_axis',(0.,0.,-1.));
#14821=DIRECTION('ref_axis',(-1.,0.,0.));
#14822=DIRECTION('',(0.,0.,-1.));
#14823=DIRECTION('center_axis',(0.,0.,-1.));
#14824=DIRECTION('ref_axis',(-0.809016994374951,0.587785252292469,0.));
#14825=DIRECTION('center_axis',(0.629320391049841,-0.777145961456968,0.));
#14826=DIRECTION('ref_axis',(0.777145961456968,0.629320391049841,0.));
#14827=DIRECTION('',(-0.777145961456968,-0.629320391049841,0.));
#14828=DIRECTION('center_axis',(-0.809016994374951,0.587785252292469,0.));
#14829=DIRECTION('ref_axis',(-0.587785252292469,-0.809016994374951,0.));
#14830=DIRECTION('center_axis',(0.809016994374951,-0.587785252292469,0.));
#14831=DIRECTION('ref_axis',(-0.587785252292469,-0.809016994374951,0.));
#14832=DIRECTION('',(0.587785252292469,0.809016994374951,0.));
#14833=DIRECTION('center_axis',(0.,-1.,0.));
#14834=DIRECTION('ref_axis',(0.,0.,-1.));
#14835=DIRECTION('',(0.,0.,-1.));
#14836=DIRECTION('',(1.,0.,0.));
#14837=DIRECTION('',(0.,0.,-1.));
#14838=DIRECTION('center_axis',(1.,0.,0.));
#14839=DIRECTION('ref_axis',(0.,0.,-1.));
#14840=DIRECTION('center_axis',(-1.,0.,0.));
#14841=DIRECTION('ref_axis',(0.,0.,-1.));
#14842=DIRECTION('',(0.,0.,-1.));
#14843=DIRECTION('',(0.,-1.,0.));
#14844=DIRECTION('center_axis',(0.,0.,-1.));
#14845=DIRECTION('ref_axis',(-1.,0.,0.));
#14846=DIRECTION('',(0.,0.,-1.));
#14847=DIRECTION('center_axis',(0.,0.,-1.));
#14848=DIRECTION('ref_axis',(-1.,0.,0.));
#14849=DIRECTION('center_axis',(0.965925826289068,-0.258819045102522,0.));
#14850=DIRECTION('ref_axis',(0.258819045102522,0.965925826289068,0.));
#14851=DIRECTION('',(-0.258819045102522,-0.965925826289068,0.));
#14852=DIRECTION('center_axis',(-1.,0.,0.));
#14853=DIRECTION('ref_axis',(0.,0.,1.));
#14854=DIRECTION('center_axis',(1.,0.,0.));
#14855=DIRECTION('ref_axis',(0.,0.,1.));
#14856=DIRECTION('',(0.,1.,0.));
#14857=DIRECTION('center_axis',(0.58778525229248,-0.809016994374942,0.));
#14858=DIRECTION('ref_axis',(0.809016994374942,0.58778525229248,0.));
#14859=DIRECTION('',(0.,0.,-1.));
#14860=DIRECTION('',(0.809016994374942,0.58778525229248,0.));
#14861=DIRECTION('',(0.,0.,-1.));
#14862=DIRECTION('center_axis',(0.809016994374942,0.58778525229248,0.));
#14863=DIRECTION('ref_axis',(-0.58778525229248,0.809016994374942,0.));
#14864=DIRECTION('center_axis',(-0.809016994374942,-0.58778525229248,0.));
#14865=DIRECTION('ref_axis',(-0.58778525229248,0.809016994374942,0.));
#14866=DIRECTION('',(0.,0.,-1.));
#14867=DIRECTION('',(0.58778525229248,-0.809016994374942,0.));
#14868=DIRECTION('center_axis',(0.,0.,-1.));
#14869=DIRECTION('ref_axis',(-1.,0.,0.));
#14870=DIRECTION('',(0.,0.,-1.));
#14871=DIRECTION('center_axis',(0.,0.,-1.));
#14872=DIRECTION('ref_axis',(-0.809016994374942,-0.58778525229248,0.));
#14873=DIRECTION('center_axis',(0.933580426497199,0.358367949545307,0.));
#14874=DIRECTION('ref_axis',(-0.358367949545307,0.933580426497199,0.));
#14875=DIRECTION('',(0.358367949545307,-0.933580426497199,0.));
#14876=DIRECTION('center_axis',(-0.809016994374942,-0.58778525229248,0.));
#14877=DIRECTION('ref_axis',(0.58778525229248,-0.809016994374942,0.));
#14878=DIRECTION('center_axis',(0.809016994374942,0.58778525229248,0.));
#14879=DIRECTION('ref_axis',(0.58778525229248,-0.809016994374942,0.));
#14880=DIRECTION('',(-0.58778525229248,0.809016994374942,0.));
#14881=DIRECTION('center_axis',(0.951056516295157,-0.309016994374938,0.));
#14882=DIRECTION('ref_axis',(0.309016994374938,0.951056516295157,0.));
#14883=DIRECTION('',(0.,0.,-1.));
#14884=DIRECTION('',(0.309016994374938,0.951056516295157,0.));
#14885=DIRECTION('',(0.,0.,-1.));
#14886=DIRECTION('center_axis',(0.309016994374938,0.951056516295157,0.));
#14887=DIRECTION('ref_axis',(-0.951056516295157,0.309016994374938,0.));
#14888=DIRECTION('center_axis',(-0.309016994374938,-0.951056516295157,0.));
#14889=DIRECTION('ref_axis',(-0.951056516295157,0.309016994374938,0.));
#14890=DIRECTION('',(0.,0.,-1.));
#14891=DIRECTION('',(0.951056516295157,-0.309016994374938,0.));
#14892=DIRECTION('center_axis',(0.,0.,-1.));
#14893=DIRECTION('ref_axis',(-1.,0.,0.));
#14894=DIRECTION('',(0.,0.,-1.));
#14895=DIRECTION('center_axis',(0.,0.,-1.));
#14896=DIRECTION('ref_axis',(-0.309016994374938,-0.951056516295157,0.));
#14897=DIRECTION('center_axis',(0.54463903501502,0.838670567945429,0.));
#14898=DIRECTION('ref_axis',(-0.838670567945428,0.54463903501502,0.));
#14899=DIRECTION('',(0.838670567945429,-0.54463903501502,0.));
#14900=DIRECTION('center_axis',(-0.309016994374938,-0.951056516295157,0.));
#14901=DIRECTION('ref_axis',(0.951056516295157,-0.309016994374938,0.));
#14902=DIRECTION('center_axis',(0.309016994374938,0.951056516295157,0.));
#14903=DIRECTION('ref_axis',(0.951056516295157,-0.309016994374938,0.));
#14904=DIRECTION('',(-0.951056516295157,0.309016994374938,0.));
#14905=DIRECTION('center_axis',(0.95105651629515,0.309016994374958,0.));
#14906=DIRECTION('ref_axis',(-0.309016994374958,0.95105651629515,0.));
#14907=DIRECTION('',(0.,0.,-1.));
#14908=DIRECTION('',(-0.309016994374958,0.95105651629515,0.));
#14909=DIRECTION('',(0.,0.,-1.));
#14910=DIRECTION('center_axis',(-0.309016994374958,0.95105651629515,0.));
#14911=DIRECTION('ref_axis',(-0.95105651629515,-0.309016994374958,0.));
#14912=DIRECTION('center_axis',(0.309016994374958,-0.95105651629515,0.));
#14913=DIRECTION('ref_axis',(-0.95105651629515,-0.309016994374958,0.));
#14914=DIRECTION('',(0.,0.,-1.));
#14915=DIRECTION('',(0.95105651629515,0.309016994374958,0.));
#14916=DIRECTION('center_axis',(0.,0.,-1.));
#14917=DIRECTION('ref_axis',(-1.,0.,0.));
#14918=DIRECTION('',(0.,0.,-1.));
#14919=DIRECTION('center_axis',(0.,0.,-1.));
#14920=DIRECTION('ref_axis',(0.309016994374958,-0.95105651629515,0.));
#14921=DIRECTION('center_axis',(-0.0523359562429538,0.998629534754573,0.));
#14922=DIRECTION('ref_axis',(-0.998629534754574,-0.0523359562429538,0.));
#14923=DIRECTION('',(0.998629534754573,0.0523359562429538,0.));
#14924=DIRECTION('center_axis',(0.309016994374958,-0.95105651629515,0.));
#14925=DIRECTION('ref_axis',(0.95105651629515,0.309016994374958,0.));
#14926=DIRECTION('center_axis',(-0.309016994374958,0.95105651629515,0.));
#14927=DIRECTION('ref_axis',(0.95105651629515,0.309016994374958,0.));
#14928=DIRECTION('',(-0.95105651629515,-0.309016994374958,0.));
#14929=DIRECTION('center_axis',(0.587785252292463,0.809016994374955,0.));
#14930=DIRECTION('ref_axis',(-0.809016994374955,0.587785252292463,0.));
#14931=DIRECTION('',(0.,0.,-1.));
#14932=DIRECTION('',(-0.809016994374955,0.587785252292463,0.));
#14933=DIRECTION('',(0.,0.,-1.));
#14934=DIRECTION('center_axis',(-0.809016994374955,0.587785252292462,0.));
#14935=DIRECTION('ref_axis',(-0.587785252292462,-0.809016994374955,0.));
#14936=DIRECTION('center_axis',(0.809016994374955,-0.587785252292462,0.));
#14937=DIRECTION('ref_axis',(-0.587785252292462,-0.809016994374955,0.));
#14938=DIRECTION('',(0.,0.,-1.));
#14939=DIRECTION('',(0.587785252292462,0.809016994374955,0.));
#14940=DIRECTION('center_axis',(0.,0.,-1.));
#14941=DIRECTION('ref_axis',(-1.,0.,0.));
#14942=DIRECTION('',(0.,0.,-1.));
#14943=DIRECTION('center_axis',(0.,0.,-1.));
#14944=DIRECTION('ref_axis',(0.809016994374955,-0.587785252292462,0.));
#14945=DIRECTION('center_axis',(-0.629320391049847,0.777145961456963,0.));
#14946=DIRECTION('ref_axis',(-0.777145961456964,-0.629320391049847,0.));
#14947=DIRECTION('',(0.777145961456963,0.629320391049847,0.));
#14948=DIRECTION('center_axis',(0.809016994374955,-0.587785252292463,0.));
#14949=DIRECTION('ref_axis',(0.587785252292463,0.809016994374955,0.));
#14950=DIRECTION('center_axis',(-0.809016994374955,0.587785252292463,0.));
#14951=DIRECTION('ref_axis',(0.587785252292463,0.809016994374955,0.));
#14952=DIRECTION('',(-0.587785252292463,-0.809016994374955,0.));
#14953=DIRECTION('center_axis',(-0.809016994374947,-0.587785252292474,0.));
#14954=DIRECTION('ref_axis',(0.587785252292474,-0.809016994374947,0.));
#14955=DIRECTION('center_axis',(-0.309016994374945,-0.951056516295155,0.));
#14956=DIRECTION('ref_axis',(0.951056516295155,-0.309016994374945,0.));
#14957=DIRECTION('center_axis',(0.309016994374952,-0.951056516295152,0.));
#14958=DIRECTION('ref_axis',(0.951056516295152,0.309016994374952,0.));
#14959=DIRECTION('center_axis',(0.809016994374951,-0.587785252292469,0.));
#14960=DIRECTION('ref_axis',(0.587785252292469,0.809016994374951,0.));
#14961=DIRECTION('center_axis',(1.,0.,0.));
#14962=DIRECTION('ref_axis',(0.,0.,-1.));
#14963=DIRECTION('center_axis',(0.809016994374942,0.58778525229248,0.));
#14964=DIRECTION('ref_axis',(-0.58778525229248,0.809016994374942,0.));
#14965=DIRECTION('center_axis',(0.309016994374938,0.951056516295157,0.));
#14966=DIRECTION('ref_axis',(-0.951056516295157,0.309016994374938,0.));
#14967=DIRECTION('center_axis',(-0.309016994374958,0.95105651629515,0.));
#14968=DIRECTION('ref_axis',(-0.95105651629515,-0.309016994374958,0.));
#14969=DIRECTION('center_axis',(-0.809016994374955,0.587785252292463,0.));
#14970=DIRECTION('ref_axis',(-0.587785252292462,-0.809016994374955,0.));
#14971=DIRECTION('center_axis',(0.,0.,1.));
#14972=DIRECTION('ref_axis',(1.,0.,0.));
#14973=DIRECTION('center_axis',(0.,0.,1.));
#14974=DIRECTION('ref_axis',(1.,0.,0.));
#14975=DIRECTION('center_axis',(0.,0.,1.));
#14976=DIRECTION('ref_axis',(1.,0.,0.));
#14977=DIRECTION('center_axis',(0.,0.,1.));
#14978=DIRECTION('ref_axis',(1.,0.,0.));
#14979=DIRECTION('center_axis',(0.,0.,1.));
#14980=DIRECTION('ref_axis',(1.,0.,0.));
#14981=DIRECTION('center_axis',(0.,0.,1.));
#14982=DIRECTION('ref_axis',(1.,0.,0.));
#14983=DIRECTION('center_axis',(0.,0.,1.));
#14984=DIRECTION('ref_axis',(1.,0.,0.));
#14985=DIRECTION('center_axis',(0.,0.,1.));
#14986=DIRECTION('ref_axis',(1.,0.,0.));
#14987=DIRECTION('center_axis',(0.,0.,1.));
#14988=DIRECTION('ref_axis',(1.,0.,0.));
#14989=DIRECTION('center_axis',(0.,0.,1.));
#14990=DIRECTION('ref_axis',(1.,0.,0.));
#14991=DIRECTION('center_axis',(0.,0.,1.));
#14992=DIRECTION('ref_axis',(1.,0.,0.));
#14993=DIRECTION('center_axis',(1.,-2.6394692217289E-16,0.));
#14994=DIRECTION('ref_axis',(2.6394692217289E-16,1.,0.));
#14995=DIRECTION('',(0.,0.,-1.));
#14996=DIRECTION('center_axis',(0.,1.,0.));
#14997=DIRECTION('ref_axis',(0.,0.,1.));
#14998=DIRECTION('',(0.,0.,-1.));
#14999=DIRECTION('center_axis',(-1.,-2.6394692217289E-16,0.));
#15000=DIRECTION('ref_axis',(2.6394692217289E-16,-1.,0.));
#15001=DIRECTION('axis',(0.,0.,1.));
#15002=DIRECTION('refdir',(1.,0.,0.));
#15003=DIRECTION('center_axis',(0.,0.,1.));
#15004=DIRECTION('ref_axis',(1.,0.,0.));
#15005=DIRECTION('center_axis',(0.,0.,1.));
#15006=DIRECTION('ref_axis',(1.,0.,0.));
#15007=DIRECTION('center_axis',(1.22464679914735E-16,-1.,0.));
#15008=DIRECTION('ref_axis',(-1.,-1.22464679914735E-16,0.));
#15009=DIRECTION('center_axis',(0.,0.,-1.));
#15010=DIRECTION('ref_axis',(1.,0.,0.));
#15011=DIRECTION('center_axis',(0.,0.,-1.));
#15012=DIRECTION('ref_axis',(1.,0.,0.));
#15013=DIRECTION('center_axis',(0.,0.,1.));
#15014=DIRECTION('ref_axis',(1.,0.,0.));
#15015=DIRECTION('center_axis',(0.,0.,1.));
#15016=DIRECTION('ref_axis',(1.,0.,0.));
#15017=DIRECTION('center_axis',(0.,0.,1.));
#15018=DIRECTION('ref_axis',(1.,0.,0.));
#15019=DIRECTION('center_axis',(1.22464679914735E-16,-1.,0.));
#15020=DIRECTION('ref_axis',(-1.,-1.22464679914735E-16,0.));
#15021=DIRECTION('center_axis',(0.,0.,-1.));
#15022=DIRECTION('ref_axis',(1.,0.,0.));
#15023=DIRECTION('center_axis',(0.,0.,1.));
#15024=DIRECTION('ref_axis',(1.,0.,0.));
#15025=DIRECTION('center_axis',(0.,0.,1.));
#15026=DIRECTION('ref_axis',(1.,0.,0.));
#15027=DIRECTION('',(-0.70710678118655,-8.65956056235496E-17,0.707106781186545));
#15028=DIRECTION('center_axis',(0.,0.,1.));
#15029=DIRECTION('ref_axis',(1.,0.,0.));
#15030=DIRECTION('center_axis',(0.,0.,1.));
#15031=DIRECTION('ref_axis',(1.,0.,0.));
#15032=DIRECTION('center_axis',(0.,0.,1.));
#15033=DIRECTION('ref_axis',(1.,0.,0.));
#15034=DIRECTION('',(0.,0.,1.));
#15035=DIRECTION('center_axis',(0.,0.,1.));
#15036=DIRECTION('ref_axis',(1.,0.,0.));
#15037=DIRECTION('center_axis',(0.,0.,1.));
#15038=DIRECTION('ref_axis',(1.,0.,0.));
#15039=DIRECTION('',(-0.70710678118655,-8.65956056235496E-17,0.707106781186545));
#15040=DIRECTION('center_axis',(0.,0.,1.));
#15041=DIRECTION('ref_axis',(1.,0.,0.));
#15042=DIRECTION('center_axis',(0.,0.,1.));
#15043=DIRECTION('ref_axis',(1.,0.,0.));
#15044=DIRECTION('center_axis',(0.,0.,1.));
#15045=DIRECTION('ref_axis',(1.,0.,0.));
#15046=DIRECTION('',(0.,0.,1.));
#15047=DIRECTION('center_axis',(0.,0.,1.));
#15048=DIRECTION('ref_axis',(1.,0.,0.));
#15049=DIRECTION('center_axis',(0.,0.,1.));
#15050=DIRECTION('ref_axis',(1.,0.,0.));
#15051=DIRECTION('',(-0.707106781186551,-8.65956056235498E-17,0.707106781186544));
#15052=DIRECTION('center_axis',(0.,0.,1.));
#15053=DIRECTION('ref_axis',(1.,0.,0.));
#15054=DIRECTION('center_axis',(0.,0.,1.));
#15055=DIRECTION('ref_axis',(1.,0.,0.));
#15056=DIRECTION('center_axis',(0.,0.,1.));
#15057=DIRECTION('ref_axis',(1.,0.,0.));
#15058=DIRECTION('',(0.,0.,1.));
#15059=DIRECTION('center_axis',(0.,0.,1.));
#15060=DIRECTION('ref_axis',(1.,0.,0.));
#15061=DIRECTION('center_axis',(0.,0.,1.));
#15062=DIRECTION('ref_axis',(1.,0.,0.));
#15063=DIRECTION('',(-0.70710678118655,-8.65956056235496E-17,0.707106781186545));
#15064=DIRECTION('center_axis',(0.,0.,1.));
#15065=DIRECTION('ref_axis',(1.,0.,0.));
#15066=DIRECTION('center_axis',(0.,0.,1.));
#15067=DIRECTION('ref_axis',(1.,0.,0.));
#15068=DIRECTION('center_axis',(0.,0.,1.));
#15069=DIRECTION('ref_axis',(1.,0.,0.));
#15070=DIRECTION('',(0.,0.,1.));
#15071=DIRECTION('center_axis',(0.,0.,1.));
#15072=DIRECTION('ref_axis',(1.,0.,0.));
#15073=DIRECTION('center_axis',(0.,0.,1.));
#15074=DIRECTION('ref_axis',(1.,0.,0.));
#15075=DIRECTION('',(-0.70710678118655,-8.65956056235496E-17,0.707106781186545));
#15076=DIRECTION('center_axis',(0.,0.,1.));
#15077=DIRECTION('ref_axis',(1.,0.,0.));
#15078=DIRECTION('center_axis',(0.,0.,1.));
#15079=DIRECTION('ref_axis',(1.,0.,0.));
#15080=DIRECTION('center_axis',(0.,0.,1.));
#15081=DIRECTION('ref_axis',(1.,0.,0.));
#15082=DIRECTION('',(0.,0.,1.));
#15083=DIRECTION('center_axis',(0.,0.,1.));
#15084=DIRECTION('ref_axis',(1.,0.,0.));
#15085=DIRECTION('center_axis',(0.,0.,1.));
#15086=DIRECTION('ref_axis',(1.,0.,0.));
#15087=DIRECTION('',(-0.707106781186551,-8.65956056235498E-17,0.707106781186544));
#15088=DIRECTION('center_axis',(0.,0.,1.));
#15089=DIRECTION('ref_axis',(1.,0.,0.));
#15090=DIRECTION('center_axis',(0.,0.,1.));
#15091=DIRECTION('ref_axis',(1.,0.,0.));
#15092=DIRECTION('center_axis',(0.,0.,1.));
#15093=DIRECTION('ref_axis',(1.,0.,0.));
#15094=DIRECTION('',(0.,0.,1.));
#15095=DIRECTION('center_axis',(0.,0.,-1.));
#15096=DIRECTION('ref_axis',(-1.,0.,0.));
#15097=DIRECTION('center_axis',(0.,0.,1.));
#15098=DIRECTION('ref_axis',(1.,0.,0.));
#15099=DIRECTION('',(0.,0.,-1.));
#15100=DIRECTION('center_axis',(0.,0.,1.));
#15101=DIRECTION('ref_axis',(1.,0.,0.));
#15102=DIRECTION('center_axis',(0.,0.,-1.));
#15103=DIRECTION('ref_axis',(-1.,0.,0.));
#15104=DIRECTION('',(0.,0.,1.));
#15105=DIRECTION('center_axis',(0.,0.,1.));
#15106=DIRECTION('ref_axis',(1.,0.,0.));
#15107=DIRECTION('center_axis',(0.,0.,1.));
#15108=DIRECTION('ref_axis',(1.,0.,0.));
#15109=DIRECTION('axis',(0.,0.,1.));
#15110=DIRECTION('refdir',(1.,0.,0.));
#15111=DIRECTION('center_axis',(0.,1.,0.));
#15112=DIRECTION('ref_axis',(0.,0.,1.));
#15113=DIRECTION('',(1.,0.,6.12323399573677E-17));
#15114=DIRECTION('',(0.,0.,1.));
#15115=DIRECTION('',(-1.,0.,0.));
#15116=DIRECTION('',(0.,0.,1.));
#15117=DIRECTION('center_axis',(1.,0.,0.));
#15118=DIRECTION('ref_axis',(0.,0.,-1.));
#15119=DIRECTION('',(0.,-1.,0.));
#15120=DIRECTION('',(0.,0.,1.));
#15121=DIRECTION('',(0.,1.,0.));
#15122=DIRECTION('center_axis',(0.,0.,1.));
#15123=DIRECTION('ref_axis',(1.,0.,0.));
#15124=DIRECTION('center_axis',(-6.12323399573677E-17,0.,1.));
#15125=DIRECTION('ref_axis',(1.,0.,6.12323399573677E-17));
#15126=DIRECTION('',(0.,0.,1.));
#15127=DIRECTION('center_axis',(0.,0.,-1.));
#15128=DIRECTION('ref_axis',(-1.,0.,0.));
#15129=DIRECTION('center_axis',(0.164410656039629,-0.986391978972162,0.));
#15130=DIRECTION('ref_axis',(0.986391978972162,0.164410656039629,0.));
#15131=DIRECTION('',(-0.986391978972162,-0.164410656039629,-6.03990889876441E-17));
#15132=DIRECTION('',(0.,0.,1.));
#15133=DIRECTION('',(0.986391978972162,0.164410656039629,0.));
#15134=DIRECTION('center_axis',(0.,0.,1.));
#15135=DIRECTION('ref_axis',(1.,0.,0.));
#15136=DIRECTION('center_axis',(6.12323399573677E-17,0.,-1.));
#15137=DIRECTION('ref_axis',(1.,-1.01179555320898E-15,6.12323399573676E-17));
#15138=DIRECTION('',(0.,0.,1.));
#15139=DIRECTION('center_axis',(0.,0.,1.));
#15140=DIRECTION('ref_axis',(-1.,0.,0.));
#15141=DIRECTION('center_axis',(1.,0.,0.));
#15142=DIRECTION('ref_axis',(0.,0.,-1.));
#15143=DIRECTION('',(0.,-1.,0.));
#15144=DIRECTION('',(0.,0.,1.));
#15145=DIRECTION('',(0.,1.,0.));
#15146=DIRECTION('center_axis',(0.,0.,1.));
#15147=DIRECTION('ref_axis',(1.,0.,0.));
#15148=DIRECTION('center_axis',(6.12323399573677E-17,0.,-1.));
#15149=DIRECTION('ref_axis',(1.,-1.01179555320898E-15,6.12323399573676E-17));
#15150=DIRECTION('',(0.,0.,1.));
#15151=DIRECTION('center_axis',(0.,0.,1.));
#15152=DIRECTION('ref_axis',(-1.,1.77064221811572E-15,0.));
#15153=DIRECTION('center_axis',(0.164410656039629,0.986391978972162,0.));
#15154=DIRECTION('ref_axis',(-0.986391978972162,0.164410656039629,0.));
#15155=DIRECTION('',(0.986391978972162,-0.164410656039629,6.03990889876441E-17));
#15156=DIRECTION('',(0.,0.,1.));
#15157=DIRECTION('',(-0.986391978972162,0.164410656039629,0.));
#15158=DIRECTION('center_axis',(0.,0.,1.));
#15159=DIRECTION('ref_axis',(1.,0.,0.));
#15160=DIRECTION('center_axis',(-6.12323399573677E-17,0.,1.));
#15161=DIRECTION('ref_axis',(1.,0.,6.12323399573677E-17));
#15162=DIRECTION('',(0.,0.,1.));
#15163=DIRECTION('center_axis',(0.,0.,-1.));
#15164=DIRECTION('ref_axis',(-1.,0.,0.));
#15165=DIRECTION('center_axis',(1.,0.,0.));
#15166=DIRECTION('ref_axis',(0.,0.,-1.));
#15167=DIRECTION('',(0.,-1.,0.));
#15168=DIRECTION('',(0.,0.,1.));
#15169=DIRECTION('',(0.,1.,0.));
#15170=DIRECTION('center_axis',(0.,-1.,0.));
#15171=DIRECTION('ref_axis',(0.,0.,-1.));
#15172=DIRECTION('',(-1.,0.,-6.12323399573677E-17));
#15173=DIRECTION('',(0.,0.,1.));
#15174=DIRECTION('',(1.,0.,0.));
#15175=DIRECTION('center_axis',(-1.,0.,0.));
#15176=DIRECTION('ref_axis',(0.,0.,1.));
#15177=DIRECTION('',(0.,1.,0.));
#15178=DIRECTION('',(0.,-1.,0.));
#15179=DIRECTION('center_axis',(0.,0.,-1.));
#15180=DIRECTION('ref_axis',(-1.,0.,0.));
#15181=DIRECTION('center_axis',(-6.12323399573677E-17,0.,1.));
#15182=DIRECTION('ref_axis',(1.,0.,6.12323399573677E-17));
#15183=DIRECTION('center_axis',(-1.,1.6672859221772E-24,-3.30995181697817E-47));
#15184=DIRECTION('ref_axis',(0.,1.98523347012726E-23,1.));
#15185=DIRECTION('',(-1.70606001339062E-24,1.,1.32348898008484E-23));
#15186=DIRECTION('center_axis',(-1.,1.6672859221772E-24,0.));
#15187=DIRECTION('ref_axis',(0.,0.,1.));
#15188=DIRECTION('',(0.,0.164410656039629,-0.986391978972162));
#15189=DIRECTION('center_axis',(1.,-1.6672859221772E-24,0.));
#15190=DIRECTION('ref_axis',(3.37390496397365E-39,2.02359110641796E-15,
1.));
#15191=DIRECTION('',(-1.70606001339062E-24,1.,1.32348898008484E-23));
#15192=DIRECTION('center_axis',(1.,-1.6672859221772E-24,0.));
#15193=DIRECTION('ref_axis',(4.63911932546376E-39,2.7824377713247E-15,1.));
#15194=DIRECTION('',(0.,0.164410656039629,0.986391978972162));
#15195=DIRECTION('center_axis',(-1.,1.6672859221772E-24,0.));
#15196=DIRECTION('ref_axis',(0.,0.,1.));
#15197=DIRECTION('',(-1.70606001339062E-24,1.,1.32348898008484E-23));
#15198=DIRECTION('',(-2.16840434497101E-19,1.98523347012726E-23,1.));
#15199=DIRECTION('',(1.70606001339062E-24,-1.,-1.32348898008484E-23));
#15200=DIRECTION('',(-2.16840434497101E-19,1.98523347012726E-23,1.));
#15201=DIRECTION('center_axis',(2.16840434497101E-19,1.98523347012726E-23,
1.));
#15202=DIRECTION('ref_axis',(1.,-2.52031592887251E-24,-2.16840434497101E-19));
#15203=DIRECTION('',(1.,-2.52031592887251E-24,-2.16840434497101E-19));
#15204=DIRECTION('',(1.70606001339062E-24,-1.,-1.32348898008484E-23));
#15205=DIRECTION('',(1.,-2.52031592887251E-24,-2.16840434497101E-19));
#15206=DIRECTION('center_axis',(1.70606001339062E-24,-1.,1.98523347012726E-23));
#15207=DIRECTION('ref_axis',(-9.11574503592928E-64,-1.98523347012726E-23,
-1.));
#15208=DIRECTION('',(1.,-2.52031592887251E-24,-2.16840434497101E-19));
#15209=DIRECTION('',(-0.198787259314375,-1.98523347012726E-23,-0.980042665160185));
#15210=DIRECTION('center_axis',(-2.16840434497101E-19,-1.98523347012726E-23,
-1.));
#15211=DIRECTION('ref_axis',(-1.,2.52031592887251E-24,2.16840434497101E-19));
#15212=DIRECTION('',(1.,-2.52031592887251E-24,-2.16840434497101E-19));
#15213=DIRECTION('',(-1.70606001339062E-24,1.,1.32348898008484E-23));
#15214=DIRECTION('center_axis',(1.,-2.52031592887251E-24,-2.16840434497101E-19));
#15215=DIRECTION('ref_axis',(-2.16840434497101E-19,5.46506401086678E-43,
-1.));
#15216=DIRECTION('',(1.,-2.52031592887251E-24,-2.16840434497101E-19));
#15217=DIRECTION('center_axis',(-0.980042665160176,-7.49762143682472E-14,
0.198787259314424));
#15218=DIRECTION('ref_axis',(0.198787259314424,-4.70069536847622E-12,0.980042665160176));
#15219=DIRECTION('center_axis',(1.0842021724855E-19,0.986391978972162,-0.164410656039629));
#15220=DIRECTION('ref_axis',(-1.44445765116552E-36,0.164410656039629,0.986391978972162));
#15221=DIRECTION('',(1.,-2.52031592887251E-24,-2.16840434497101E-19));
#15222=DIRECTION('',(0.196186965810001,0.161215582689263,0.967222937250987));
#15223=DIRECTION('center_axis',(1.,-2.52031592887251E-24,-2.16840434497101E-19));
#15224=DIRECTION('ref_axis',(-2.16840434497101E-19,5.46506401086678E-43,
-1.));
#15225=DIRECTION('',(1.,-2.52031592887251E-24,-2.16840434497101E-19));
#15226=DIRECTION('center_axis',(0.980042665160181,4.41011730354711E-14,
-0.198787259314396));
#15227=DIRECTION('ref_axis',(0.198787259314396,-7.64602919273965E-13,0.980042665160181));
#15228=DIRECTION('center_axis',(-2.16840434497101E-19,-1.98523347012726E-23,
-1.));
#15229=DIRECTION('ref_axis',(-1.,2.52031592887251E-24,2.16840434497101E-19));
#15230=DIRECTION('',(1.,-2.52031592887251E-24,-2.16840434497101E-19));
#15231=DIRECTION('',(-1.70606001339062E-24,1.,1.32348898008484E-23));
#15232=DIRECTION('center_axis',(1.,-2.52031592887251E-24,-2.16840434497101E-19));
#15233=DIRECTION('ref_axis',(-2.16840434497101E-19,5.46506401086678E-43,
-1.));
#15234=DIRECTION('',(1.,-2.52031592887251E-24,-2.16840434497101E-19));
#15235=DIRECTION('center_axis',(0.980042665160188,1.60789922741767E-14,
-0.198787259314364));
#15236=DIRECTION('ref_axis',(0.198787259314364,7.36955750229359E-12,0.980042665160188));
#15237=DIRECTION('center_axis',(1.0842021724855E-19,-0.986391978972162,
-0.164410656039629));
#15238=DIRECTION('ref_axis',(2.16840434497101E-19,0.164410656039629,-0.986391978972162));
#15239=DIRECTION('',(1.,-2.52031592887251E-24,-2.16840434497101E-19));
#15240=DIRECTION('',(-0.196186965810001,0.161215582689263,-0.967222937250987));
#15241=DIRECTION('center_axis',(1.,-2.52031592887251E-24,-2.16840434497101E-19));
#15242=DIRECTION('ref_axis',(-2.16840434497101E-19,5.46506401086678E-43,
-1.));
#15243=DIRECTION('',(1.,-2.52031592887251E-24,-2.16840434497101E-19));
#15244=DIRECTION('center_axis',(-0.980042665160195,-9.32929719057768E-14,
0.198787259314327));
#15245=DIRECTION('ref_axis',(0.198787259314327,2.85203844610398E-12,0.980042665160195));
#15246=DIRECTION('center_axis',(-2.16840434497101E-19,-1.98523347012726E-23,
-1.));
#15247=DIRECTION('ref_axis',(-1.,2.52031592887251E-24,2.16840434497101E-19));
#15248=DIRECTION('',(1.,-2.52031592887251E-24,-2.16840434497101E-19));
#15249=DIRECTION('',(-1.70606001339062E-24,1.,1.32348898008484E-23));
#15250=DIRECTION('center_axis',(-1.70606001339062E-24,1.,-1.98523347012726E-23));
#15251=DIRECTION('ref_axis',(9.11574503592928E-64,1.98523347012726E-23,
1.));
#15252=DIRECTION('',(0.198787259314375,1.98523347012726E-23,0.980042665160185));
#15253=DIRECTION('center_axis',(-0.980042665160186,8.27180612553027E-24,
0.198787259314375));
#15254=DIRECTION('ref_axis',(0.198787259314375,1.98523347012726E-23,0.980042665160185));
#15255=DIRECTION('center_axis',(-0.980042665160186,-3.47415857272272E-23,
0.198787259314375));
#15256=DIRECTION('ref_axis',(0.198787259314375,-6.61744490042422E-24,0.980042665160185));
#15257=DIRECTION('',(2.40300129244162E-15,1.,1.18470558471201E-14));
#15258=DIRECTION('',(-0.198787259314375,6.79161872365112E-15,-0.980042665160185));
#15259=DIRECTION('',(-1.45507196095848E-15,-1.,-7.17366179404169E-15));
#15260=DIRECTION('',(0.198787259314375,-6.79161872365112E-15,0.980042665160185));
#15261=DIRECTION('',(3.30872245021211E-23,1.,-1.32348898008484E-23));
#15262=DIRECTION('center_axis',(-0.980042665160169,5.02500160127644E-14,
0.198787259314459));
#15263=DIRECTION('ref_axis',(0.198787259314459,7.90533358256112E-12,0.980042665160169));
#15264=DIRECTION('',(-0.196186965810001,0.161215582689269,-0.967222937250986));
#15265=DIRECTION('center_axis',(0.980042665160191,2.27047187493627E-14,
-0.198787259314346));
#15266=DIRECTION('ref_axis',(0.198787259314346,3.87807928502627E-12,0.980042665160191));
#15267=DIRECTION('',(1.54401270509304E-15,1.,7.61214923421315E-15));
#15268=DIRECTION('center_axis',(0.980042665160188,-1.48340309301132E-14,
-0.198787259314363));
#15269=DIRECTION('ref_axis',(0.198787259314363,-3.96081673643786E-12,0.980042665160188));
#15270=DIRECTION('',(0.196186965810001,0.161215582689256,0.967222937250988));
#15271=DIRECTION('center_axis',(-0.980042665160184,-1.70918421812105E-14,
0.198787259314383));
#15272=DIRECTION('ref_axis',(0.198787259314383,-4.35767870224177E-11,0.980042665160184));
#15273=DIRECTION('center_axis',(0.389639990836698,-7.17366180396786E-15,
0.920967251068559));
#15274=DIRECTION('ref_axis',(0.920967251068559,2.57459965496616E-23,-0.389639990836698));
#15275=DIRECTION('',(-0.920967251068559,-2.65990265724083E-23,0.389639990836698));
#15276=DIRECTION('',(-1.45507196095848E-15,-1.,-7.17366179404169E-15));
#15277=DIRECTION('',(-0.920967251068559,-2.65990265724083E-23,0.389639990836698));
#15278=DIRECTION('center_axis',(2.70017457815614E-15,1.,6.38223076123854E-15));
#15279=DIRECTION('ref_axis',(-2.22044604925031E-16,-6.38223076123854E-15,
1.));
#15280=DIRECTION('',(0.198787259314375,-6.79161872365112E-15,0.980042665160185));
#15281=DIRECTION('',(-0.920967251068559,-2.65990265724083E-23,0.389639990836698));
#15282=DIRECTION('center_axis',(-0.389639990836698,-7.3468396926393E-39,
-0.920967251068559));
#15283=DIRECTION('ref_axis',(-0.920967251068559,-2.65990265724083E-23,0.389639990836698));
#15284=DIRECTION('',(3.30872245021211E-23,1.,-1.32348898008484E-23));
#15285=DIRECTION('',(-0.920967251068559,-2.65990265724083E-23,0.389639990836698));
#15286=DIRECTION('center_axis',(-0.920967251068559,-2.65990265724083E-23,
0.389639990836698));
#15287=DIRECTION('ref_axis',(0.389639990836698,2.27914651832168E-37,0.920967251068559));
#15288=DIRECTION('center_axis',(-0.980042665160215,-1.25938390471903E-13,
0.19878725931423));
#15289=DIRECTION('ref_axis',(0.19878725931423,2.5853135894082E-11,0.980042665160215));
#15290=DIRECTION('',(-0.920967251068559,-2.65990265724083E-23,0.389639990836698));
#15291=DIRECTION('center_axis',(-0.0640609665127394,-0.986391978972161,
-0.151416829939202));
#15292=DIRECTION('ref_axis',(3.8859753641063E-16,0.151728482244607,-0.988422211241607));
#15293=DIRECTION('',(-0.196186965810001,0.161215582689269,-0.967222937250986));
#15294=DIRECTION('',(-0.920967251068559,-2.65990265724083E-23,0.389639990836698));
#15295=DIRECTION('center_axis',(-0.920967251068559,-2.65990265724083E-23,
0.389639990836698));
#15296=DIRECTION('ref_axis',(0.389639990836698,5.40790242502236E-38,0.920967251068559));
#15297=DIRECTION('center_axis',(0.980042665160185,-4.60002666111622E-15,
-0.198787259314377));
#15298=DIRECTION('ref_axis',(0.198787259314377,2.73860543621281E-12,0.980042665160185));
#15299=DIRECTION('',(-0.920967251068559,-2.65990265724083E-23,0.389639990836698));
#15300=DIRECTION('center_axis',(-0.389639990836698,7.61214924744803E-15,
-0.920967251068559));
#15301=DIRECTION('ref_axis',(-0.920967251068559,-2.6599026609348E-23,0.389639990836698));
#15302=DIRECTION('',(1.54401270509304E-15,1.,7.61214923421315E-15));
#15303=DIRECTION('',(-0.920967251068559,-2.65990265724083E-23,0.389639990836698));
#15304=DIRECTION('center_axis',(-0.920967251068559,-2.65990265724083E-23,
0.389639990836698));
#15305=DIRECTION('ref_axis',(0.389639990836698,3.20788036696344E-38,0.920967251068559));
#15306=DIRECTION('center_axis',(0.980042665160175,4.09782191554472E-14,
-0.198787259314427));
#15307=DIRECTION('ref_axis',(0.198787259314427,-1.19923446014724E-11,0.980042665160175));
#15308=DIRECTION('',(-0.920967251068559,-2.65990265724083E-23,0.389639990836698));
#15309=DIRECTION('center_axis',(-0.0640609665127342,0.986391978972163,-0.15141682993919));
#15310=DIRECTION('ref_axis',(-2.80362758003424E-16,0.151728482244595,0.988422211241609));
#15311=DIRECTION('',(0.196186965810001,0.161215582689256,0.967222937250988));
#15312=DIRECTION('',(-0.920967251068559,-2.65990265724083E-23,0.389639990836698));
#15313=DIRECTION('center_axis',(-0.920967251068559,-2.65990265724083E-23,
0.389639990836698));
#15314=DIRECTION('ref_axis',(0.389639990836698,2.27914651832168E-37,0.920967251068559));
#15315=DIRECTION('center_axis',(-0.980042665160188,-5.1617363387258E-14,
0.198787259314362));
#15316=DIRECTION('ref_axis',(0.198787259314362,4.05302242487948E-11,0.980042665160188));
#15317=DIRECTION('',(-0.920967251068559,-2.65990265724083E-23,0.389639990836698));
#15318=DIRECTION('center_axis',(-0.389639990836698,1.18470558636637E-14,
-0.920967251068559));
#15319=DIRECTION('ref_axis',(-0.920967251068559,-2.6599026296095E-23,0.389639990836698));
#15320=DIRECTION('',(2.40300129244162E-15,1.,1.18470558471201E-14));
#15321=DIRECTION('',(-0.920967251068559,-2.65990265724083E-23,0.389639990836698));
#15322=DIRECTION('center_axis',(-2.70017457815614E-15,-1.,-6.38223076123854E-15));
#15323=DIRECTION('ref_axis',(2.22044604925031E-16,6.38223076123854E-15,
-1.));
#15324=DIRECTION('',(-0.198787259314375,6.79161872365112E-15,-0.980042665160185));
#15325=DIRECTION('center_axis',(-0.980042665160186,-5.12851979782877E-23,
0.198787259314375));
#15326=DIRECTION('ref_axis',(0.198787259314375,-6.61744490042422E-24,0.980042665160185));
#15327=DIRECTION('center_axis',(5.76441489372891E-24,-1.,-6.92992146256797E-15));
#15328=DIRECTION('ref_axis',(1.3010426069826E-18,6.92992146256797E-15,-1.));
#15329=DIRECTION('',(1.3010426069826E-18,-1.98523347012727E-23,-1.));
#15330=DIRECTION('',(-1.,3.41212002678124E-24,8.67361737988404E-19));
#15331=DIRECTION('',(-0.198787259314375,6.79161869718135E-15,-0.980042665160185));
#15332=DIRECTION('',(-1.,3.41212002678124E-24,8.67361737988404E-19));
#15333=DIRECTION('center_axis',(1.3010426069826E-18,1.18470558768986E-14,
-1.));
#15334=DIRECTION('ref_axis',(-5.81611368201347E-24,1.,1.18470558768986E-14));
#15335=DIRECTION('',(5.81611368201347E-24,-1.,-1.18470558768986E-14));
#15336=DIRECTION('',(2.40300126044007E-15,1.,1.18470558768986E-14));
#15337=DIRECTION('',(-1.,3.41212002678124E-24,8.67361737988404E-19));
#15338=DIRECTION('center_axis',(-1.,3.41212002678124E-24,8.67361737988404E-19));
#15339=DIRECTION('ref_axis',(8.67361737988404E-19,-2.95954235665401E-42,
1.));
#15340=DIRECTION('center_axis',(1.,-3.41212002678124E-24,-8.67361737988404E-19));
#15341=DIRECTION('ref_axis',(-8.67361737988404E-19,2.95954235665401E-42,
-1.));
#15342=DIRECTION('center_axis',(-0.980042665160201,6.09039309723804E-14,
0.198787259314301));
#15343=DIRECTION('ref_axis',(0.198787259314301,1.98355794240169E-13,0.9800426651602));
#15344=DIRECTION('',(-1.,3.41212002678124E-24,8.67361737988404E-19));
#15345=DIRECTION('center_axis',(5.42101086242754E-20,0.986391978972163,
-0.164410656039623));
#15346=DIRECTION('ref_axis',(-1.3010426069826E-18,0.164410656039623,0.986391978972163));
#15347=DIRECTION('',(1.3010426069826E-18,-0.164410656039623,-0.986391978972163));
#15348=DIRECTION('',(0.196186965810001,0.161215582689256,0.967222937250988));
#15349=DIRECTION('',(-1.,3.41212002678124E-24,8.67361737988404E-19));
#15350=DIRECTION('center_axis',(-1.,3.41212002678124E-24,8.67361737988404E-19));
#15351=DIRECTION('ref_axis',(8.67361737988404E-19,-2.95954235665401E-42,
1.));
#15352=DIRECTION('center_axis',(-1.,3.41212002678124E-24,8.67361737988404E-19));
#15353=DIRECTION('ref_axis',(-8.67361737988404E-19,-2.30183488355044E-14,
-1.));
#15354=DIRECTION('center_axis',(0.980042665160188,-1.44120101355155E-14,
-0.198787259314364));
#15355=DIRECTION('ref_axis',(0.198787259314364,9.45740959535352E-13,0.980042665160188));
#15356=DIRECTION('',(-1.,3.41212002678124E-24,8.67361737988404E-19));
#15357=DIRECTION('center_axis',(1.3010426069826E-18,7.61214926068292E-15,
-1.));
#15358=DIRECTION('ref_axis',(-6.15215580586314E-24,1.,7.61214926068292E-15));
#15359=DIRECTION('',(6.15215580586314E-24,-1.,-7.61214926068292E-15));
#15360=DIRECTION('',(1.54401265703901E-15,1.,7.61214926730037E-15));
#15361=DIRECTION('',(-1.,3.41212002678124E-24,8.67361737988404E-19));
#15362=DIRECTION('center_axis',(-1.,3.41212002678124E-24,8.67361737988404E-19));
#15363=DIRECTION('ref_axis',(8.67361737988404E-19,-2.95954235665401E-42,
1.));
#15364=DIRECTION('center_axis',(-1.,3.41212002678124E-24,8.67361737988404E-19));
#15365=DIRECTION('ref_axis',(-8.67361737988404E-19,-1.01179555320898E-15,
-1.));
#15366=DIRECTION('center_axis',(0.980042665160185,-5.02204745571411E-15,
-0.198787259314378));
#15367=DIRECTION('ref_axis',(0.198787259314378,7.98881519935689E-12,0.980042665160185));
#15368=DIRECTION('',(-1.,3.41212002678124E-24,8.67361737988404E-19));
#15369=DIRECTION('center_axis',(2.40741243048404E-35,-0.986391978972161,
-0.164410656039636));
#15370=DIRECTION('ref_axis',(4.33680868994201E-19,0.164410656039636,-0.986391978972161));
#15371=DIRECTION('',(-4.33680868994201E-19,-0.164410656039636,0.986391978972161));
#15372=DIRECTION('',(-0.196186965810001,0.161215582689269,-0.967222937250986));
#15373=DIRECTION('',(-1.,3.41212002678124E-24,8.67361737988404E-19));
#15374=DIRECTION('center_axis',(-1.,3.41212002678124E-24,8.67361737988404E-19));
#15375=DIRECTION('ref_axis',(8.67361737988404E-19,-2.95954235665401E-42,
1.));
#15376=DIRECTION('center_axis',(1.,-3.41212002678124E-24,-8.67361737988404E-19));
#15377=DIRECTION('ref_axis',(-8.67361737988404E-19,2.95954235665401E-42,
-1.));
#15378=DIRECTION('center_axis',(-0.980042665160198,-4.68316475765215E-14,
0.198787259314315));
#15379=DIRECTION('ref_axis',(0.198787259314315,-2.51180706998856E-11,0.980042665160198));
#15380=DIRECTION('',(-1.,3.41212002678124E-24,8.67361737988404E-19));
#15381=DIRECTION('center_axis',(-8.67361737988404E-19,-1.98523347012726E-23,
-1.));
#15382=DIRECTION('ref_axis',(-1.,3.41212002678124E-24,8.67361737988404E-19));
#15383=DIRECTION('',(3.43796942092352E-24,-1.,-1.98523347012727E-23));
#15384=DIRECTION('',(-3.43796942092352E-24,1.,1.98523347012727E-23));
#15385=DIRECTION('',(-1.,3.41212002678124E-24,8.67361737988404E-19));
#15386=DIRECTION('center_axis',(-5.76441489372891E-24,1.,6.92992146256797E-15));
#15387=DIRECTION('ref_axis',(-1.3010426069826E-18,-6.92992146256797E-15,
1.));
#15388=DIRECTION('',(1.3010426069826E-18,-1.98523347012727E-23,-1.));
#15389=DIRECTION('',(0.198787259314375,-6.79161869718135E-15,0.980042665160185));
#15390=DIRECTION('',(-1.,3.41212002678124E-24,8.67361737988404E-19));
#15391=DIRECTION('center_axis',(-1.3010426069826E-18,-7.17366181720274E-15,
1.));
#15392=DIRECTION('ref_axis',(5.97121004686716E-24,-1.,-7.17366181720274E-15));
#15393=DIRECTION('',(-5.97121004686716E-24,1.,7.17366181720274E-15));
#15394=DIRECTION('',(-1.4550719198321E-15,-1.,-7.17366180396785E-15));
#15395=DIRECTION('center_axis',(-0.980042665160186,1.32348898008484E-23,
0.198787259314375));
#15396=DIRECTION('ref_axis',(0.198787259314375,1.98523347012727E-23,0.980042665160185));
#15397=DIRECTION('center_axis',(1.,-3.41212002678124E-24,1.3010426069826E-18));
#15398=DIRECTION('ref_axis',(1.3010426069826E-18,-1.98523347012726E-23,
-1.));
#15399=DIRECTION('center_axis',(0.,1.,0.));
#15400=DIRECTION('ref_axis',(0.,0.,1.));
#15401=DIRECTION('',(-1.,0.,-5.55111512312578E-17));
#15402=DIRECTION('',(0.,0.,-1.));
#15403=DIRECTION('',(1.,0.,-5.55111512312578E-17));
#15404=DIRECTION('',(0.,0.,-1.));
#15405=DIRECTION('center_axis',(-1.,0.,0.));
#15406=DIRECTION('ref_axis',(0.,0.,1.));
#15407=DIRECTION('',(0.,-1.,0.));
#15408=DIRECTION('',(0.,0.,-1.));
#15409=DIRECTION('',(0.,1.,0.));
#15410=DIRECTION('center_axis',(0.,0.,-1.));
#15411=DIRECTION('ref_axis',(-1.,0.,0.));
#15412=DIRECTION('center_axis',(5.55111512312578E-17,0.,-1.));
#15413=DIRECTION('ref_axis',(-1.,0.,-5.55111512312578E-17));
#15414=DIRECTION('',(0.,0.,-1.));
#15415=DIRECTION('center_axis',(5.55111512312578E-17,0.,1.));
#15416=DIRECTION('ref_axis',(1.,0.,-5.55111512312578E-17));
#15417=DIRECTION('center_axis',(-0.164410656039629,-0.986391978972162,0.));
#15418=DIRECTION('ref_axis',(0.986391978972162,-0.164410656039629,0.));
#15419=DIRECTION('',(0.986391978972162,-0.164410656039629,5.47557543180234E-17));
#15420=DIRECTION('',(0.,0.,-1.));
#15421=DIRECTION('',(-0.986391978972162,0.164410656039629,5.47557543180234E-17));
#15422=DIRECTION('center_axis',(0.,0.,-1.));
#15423=DIRECTION('ref_axis',(-1.,0.,0.));
#15424=DIRECTION('center_axis',(-5.55111512312578E-17,0.,1.));
#15425=DIRECTION('ref_axis',(-1.,-1.011795553209E-15,-5.55111512312578E-17));
#15426=DIRECTION('',(0.,0.,-1.));
#15427=DIRECTION('center_axis',(-5.55111512312578E-17,0.,-1.));
#15428=DIRECTION('ref_axis',(1.,0.,-5.55111512312578E-17));
#15429=DIRECTION('center_axis',(-1.,0.,0.));
#15430=DIRECTION('ref_axis',(0.,0.,1.));
#15431=DIRECTION('',(0.,-1.,0.));
#15432=DIRECTION('',(0.,0.,-1.));
#15433=DIRECTION('',(0.,1.,0.));
#15434=DIRECTION('center_axis',(0.,0.,-1.));
#15435=DIRECTION('ref_axis',(-1.,0.,0.));
#15436=DIRECTION('center_axis',(-5.55111512312578E-17,0.,1.));
#15437=DIRECTION('ref_axis',(-1.,5.31192665434724E-15,-5.55111512312578E-17));
#15438=DIRECTION('',(0.,0.,-1.));
#15439=DIRECTION('center_axis',(-5.55111512312578E-17,0.,-1.));
#15440=DIRECTION('ref_axis',(1.,1.77064221811575E-15,-5.55111512312578E-17));
#15441=DIRECTION('center_axis',(-0.164410656039629,0.986391978972162,0.));
#15442=DIRECTION('ref_axis',(-0.986391978972162,-0.164410656039629,0.));
#15443=DIRECTION('',(-0.986391978972162,-0.164410656039629,-5.47557543180234E-17));
#15444=DIRECTION('',(0.,0.,-1.));
#15445=DIRECTION('',(0.986391978972162,0.164410656039629,-5.47557543180234E-17));
#15446=DIRECTION('center_axis',(0.,0.,-1.));
#15447=DIRECTION('ref_axis',(-1.,0.,0.));
#15448=DIRECTION('center_axis',(5.55111512312578E-17,0.,-1.));
#15449=DIRECTION('ref_axis',(-1.,0.,-5.55111512312578E-17));
#15450=DIRECTION('',(0.,0.,-1.));
#15451=DIRECTION('center_axis',(5.55111512312578E-17,0.,1.));
#15452=DIRECTION('ref_axis',(1.,0.,-5.55111512312578E-17));
#15453=DIRECTION('center_axis',(-1.,0.,0.));
#15454=DIRECTION('ref_axis',(0.,0.,1.));
#15455=DIRECTION('',(0.,-1.,0.));
#15456=DIRECTION('',(0.,0.,-1.));
#15457=DIRECTION('',(0.,1.,0.));
#15458=DIRECTION('center_axis',(0.,-1.,0.));
#15459=DIRECTION('ref_axis',(0.,0.,-1.));
#15460=DIRECTION('',(1.,0.,5.55111512312578E-17));
#15461=DIRECTION('',(0.,0.,-1.));
#15462=DIRECTION('',(-1.,0.,5.55111512312578E-17));
#15463=DIRECTION('center_axis',(1.,0.,0.));
#15464=DIRECTION('ref_axis',(0.,0.,-1.));
#15465=DIRECTION('',(0.,1.,0.));
#15466=DIRECTION('',(0.,-1.,0.));
#15467=DIRECTION('center_axis',(5.55111512312578E-17,0.,1.));
#15468=DIRECTION('ref_axis',(1.,0.,-5.55111512312578E-17));
#15469=DIRECTION('center_axis',(5.55111512312578E-17,0.,-1.));
#15470=DIRECTION('ref_axis',(-1.,0.,-5.55111512312578E-17));
#15471=DIRECTION('center_axis',(-1.,5.97767239540274E-24,-8.67361737988403E-19));
#15472=DIRECTION('ref_axis',(-8.67361737988403E-19,6.61744490042422E-24,
1.));
#15473=DIRECTION('',(6.81131535649133E-24,-1.,6.61744490042422E-24));
#15474=DIRECTION('',(-4.33680868994202E-19,1.98523347012727E-23,1.));
#15475=DIRECTION('',(-6.81131535649133E-24,1.,-6.61744490042422E-24));
#15476=DIRECTION('',(-4.33680868994202E-19,1.98523347012727E-23,1.));
#15477=DIRECTION('',(6.81131535649133E-24,-1.,6.61744490042422E-24));
#15478=DIRECTION('center_axis',(-1.,5.97767239540274E-24,6.50521303491302E-19));
#15479=DIRECTION('ref_axis',(6.50521303491302E-19,-3.88860323850136E-42,
1.));
#15480=DIRECTION('',(-8.67361737988403E-19,-0.164410656039629,0.986391978972162));
#15481=DIRECTION('center_axis',(1.,-5.97767239540274E-24,-6.50521303491302E-19));
#15482=DIRECTION('ref_axis',(6.50521303491302E-19,-3.88860323850136E-42,
1.));
#15483=DIRECTION('',(6.81131535649133E-24,-1.,6.61744490042422E-24));
#15484=DIRECTION('center_axis',(1.,-5.97767239540274E-24,-6.50521303491302E-19));
#15485=DIRECTION('ref_axis',(6.50521303491302E-19,-2.02359110641796E-15,
1.));
#15486=DIRECTION('',(1.51788304147971E-18,-0.164410656039629,-0.986391978972162));
#15487=DIRECTION('center_axis',(-1.,5.97767239540274E-24,6.50521303491302E-19));
#15488=DIRECTION('ref_axis',(6.50521303491302E-19,-3.88860323850136E-42,
1.));
#15489=DIRECTION('center_axis',(-6.50521303491302E-19,-6.61744490042422E-24,
-1.));
#15490=DIRECTION('ref_axis',(-1.,5.97767239540274E-24,6.50521303491302E-19));
#15491=DIRECTION('',(-1.,5.97767239540274E-24,6.50521303491302E-19));
#15492=DIRECTION('',(-6.81131535649133E-24,1.,-6.61744490042422E-24));
#15493=DIRECTION('',(-1.,5.97767239540274E-24,6.50521303491302E-19));
#15494=DIRECTION('center_axis',(6.81131535649133E-24,-1.,6.61744490042422E-24));
#15495=DIRECTION('ref_axis',(8.67361737988403E-19,-6.61744490042422E-24,
-1.));
#15496=DIRECTION('',(0.198787259314375,-6.61744490042422E-24,-0.980042665160185));
#15497=DIRECTION('',(-1.,5.97767239540274E-24,6.50521303491302E-19));
#15498=DIRECTION('center_axis',(6.50521303491302E-19,6.61744490042422E-24,
1.));
#15499=DIRECTION('ref_axis',(1.,-5.97767239540274E-24,-6.50521303491302E-19));
#15500=DIRECTION('',(6.81131535649133E-24,-1.,6.61744490042422E-24));
#15501=DIRECTION('',(-1.,5.97767239540274E-24,6.50521303491302E-19));
#15502=DIRECTION('center_axis',(-1.,5.97767239540274E-24,6.50521303491302E-19));
#15503=DIRECTION('ref_axis',(6.50521303491302E-19,-3.88860323850136E-42,
1.));
#15504=DIRECTION('center_axis',(-0.980042665160172,-3.50952492787524E-14,
-0.198787259314441));
#15505=DIRECTION('ref_axis',(0.198787259314441,-1.6456332591569E-11,-0.980042665160172));
#15506=DIRECTION('',(-1.,5.97767239540274E-24,6.50521303491302E-19));
#15507=DIRECTION('center_axis',(-1.0842021724855E-19,0.986391978972162,
0.16441065603963));
#15508=DIRECTION('ref_axis',(-6.50521303491303E-19,-0.164410656039629,0.986391978972162));
#15509=DIRECTION('',(-0.196186965810001,-0.161215582689263,0.967222937250987));
#15510=DIRECTION('',(-1.,5.97767239540274E-24,6.50521303491302E-19));
#15511=DIRECTION('center_axis',(-1.,5.97767239540274E-24,6.50521303491302E-19));
#15512=DIRECTION('ref_axis',(6.50521303491302E-19,-3.88860323850136E-42,
1.));
#15513=DIRECTION('center_axis',(0.980042665160175,3.79396694343426E-14,
0.198787259314425));
#15514=DIRECTION('ref_axis',(0.198787259314425,3.87086750237462E-12,-0.980042665160175));
#15515=DIRECTION('',(-1.,5.97767239540274E-24,6.50521303491302E-19));
#15516=DIRECTION('center_axis',(6.50521303491302E-19,6.61744490042422E-24,
1.));
#15517=DIRECTION('ref_axis',(1.,-5.97767239540274E-24,-6.50521303491302E-19));
#15518=DIRECTION('',(6.81131535649133E-24,-1.,6.61744490042422E-24));
#15519=DIRECTION('',(-1.,5.97767239540274E-24,6.50521303491302E-19));
#15520=DIRECTION('center_axis',(-1.,5.97767239540274E-24,6.50521303491302E-19));
#15521=DIRECTION('ref_axis',(6.50521303491302E-19,-3.88860323850136E-42,
1.));
#15522=DIRECTION('center_axis',(0.980042665160169,-9.74657025123624E-14,
0.198787259314457));
#15523=DIRECTION('ref_axis',(0.198787259314457,9.35920069890102E-12,-0.980042665160169));
#15524=DIRECTION('',(-1.,5.97767239540274E-24,6.50521303491302E-19));
#15525=DIRECTION('center_axis',(-3.79470760369927E-19,-0.986391978972162,
0.164410656039629));
#15526=DIRECTION('ref_axis',(1.51788304147971E-18,-0.164410656039629,-0.986391978972162));
#15527=DIRECTION('',(0.196186965810001,-0.161215582689263,-0.967222937250987));
#15528=DIRECTION('',(-1.,5.97767239540274E-24,6.50521303491302E-19));
#15529=DIRECTION('center_axis',(-1.,5.97767239540274E-24,6.50521303491302E-19));
#15530=DIRECTION('ref_axis',(6.50521303491302E-19,-3.88860323850136E-42,
1.));
#15531=DIRECTION('center_axis',(-0.980042665160186,-2.44983071264037E-14,
-0.198787259314374));
#15532=DIRECTION('ref_axis',(0.198787259314374,-1.03406121780998E-11,-0.980042665160186));
#15533=DIRECTION('',(-1.,5.97767239540274E-24,6.50521303491302E-19));
#15534=DIRECTION('center_axis',(6.50521303491302E-19,6.61744490042422E-24,
1.));
#15535=DIRECTION('ref_axis',(1.,-5.97767239540274E-24,-6.50521303491302E-19));
#15536=DIRECTION('',(6.81131535649133E-24,-1.,6.61744490042422E-24));
#15537=DIRECTION('',(-1.,5.97767239540274E-24,6.50521303491302E-19));
#15538=DIRECTION('center_axis',(-6.81131535649133E-24,1.,-6.61744490042422E-24));
#15539=DIRECTION('ref_axis',(-8.67361737988403E-19,6.61744490042422E-24,
1.));
#15540=DIRECTION('',(-0.198787259314375,6.61744490042422E-24,0.980042665160185));
#15541=DIRECTION('center_axis',(-0.980042665160186,4.96308367531816E-24,
-0.198787259314375));
#15542=DIRECTION('ref_axis',(-0.198787259314375,6.61744490042422E-24,0.980042665160185));
#15543=DIRECTION('center_axis',(1.08050467514739E-23,1.,-1.32348898008484E-23));
#15544=DIRECTION('ref_axis',(3.46944695195361E-18,1.32348898008484E-23,
1.));
#15545=DIRECTION('',(-0.198787259314375,1.98523347012726E-23,0.980042665160185));
#15546=DIRECTION('',(-1.,-1.07791973573316E-23,-1.30104260698261E-18));
#15547=DIRECTION('',(-3.46944695195361E-18,-1.32348898008484E-23,-1.));
#15548=DIRECTION('',(-1.,-1.07791973573316E-23,-1.30104260698261E-18));
#15549=DIRECTION('center_axis',(-1.3010426069826E-18,1.32348898008484E-23,
1.));
#15550=DIRECTION('ref_axis',(1.,1.07791973573316E-23,1.3010426069826E-18));
#15551=DIRECTION('',(-1.08050467514739E-23,-1.,-1.32348898008484E-23));
#15552=DIRECTION('',(-1.,-1.07791973573316E-23,-1.30104260698261E-18));
#15553=DIRECTION('',(1.08050467514739E-23,1.,1.32348898008484E-23));
#15554=DIRECTION('center_axis',(-1.,-1.07791973573316E-23,-1.3010426069826E-18));
#15555=DIRECTION('ref_axis',(-1.3010426069826E-18,-1.40241950309628E-41,
1.));
#15556=DIRECTION('center_axis',(-0.980042665160171,3.72032431477704E-14,
-0.198787259314447));
#15557=DIRECTION('ref_axis',(0.198787259314447,2.49978107929975E-11,-0.980042665160171));
#15558=DIRECTION('',(-1.,-1.07791973573316E-23,-1.30104260698261E-18));
#15559=DIRECTION('center_axis',(1.,1.07791973573316E-23,1.3010426069826E-18));
#15560=DIRECTION('ref_axis',(1.30104260698261E-18,1.40241950309628E-41,
-1.));
#15561=DIRECTION('center_axis',(4.87890977618476E-19,-0.986391978972162,
0.164410656039629));
#15562=DIRECTION('ref_axis',(-3.46944695195361E-18,-0.164410656039629,-0.986391978972162));
#15563=DIRECTION('',(0.196186965810001,-0.161215582689263,-0.967222937250987));
#15564=DIRECTION('',(-1.,-1.07791973573316E-23,-1.30104260698261E-18));
#15565=DIRECTION('',(3.46944695195361E-18,0.164410656039629,0.986391978972162));
#15566=DIRECTION('center_axis',(-1.,-1.07791973573316E-23,-1.3010426069826E-18));
#15567=DIRECTION('ref_axis',(-1.3010426069826E-18,-1.40241950309628E-41,
1.));
#15568=DIRECTION('center_axis',(0.98004266516019,3.28754198991703E-14,0.198787259314354));
#15569=DIRECTION('ref_axis',(0.198787259314354,8.48405160975645E-13,-0.98004266516019));
#15570=DIRECTION('',(-1.,-1.07791973573316E-23,-1.30104260698261E-18));
#15571=DIRECTION('center_axis',(-1.,-1.07791973573316E-23,-1.3010426069826E-18));
#15572=DIRECTION('ref_axis',(1.3010426069826E-18,1.01179555320898E-15,-1.));
#15573=DIRECTION('center_axis',(-1.3010426069826E-18,1.32348898008484E-23,
1.));
#15574=DIRECTION('ref_axis',(1.,1.07791973573316E-23,1.3010426069826E-18));
#15575=DIRECTION('',(-1.08050467514739E-23,-1.,-1.32348898008484E-23));
#15576=DIRECTION('',(-1.,-1.07791973573316E-23,-1.30104260698261E-18));
#15577=DIRECTION('',(1.08050467514739E-23,1.,1.32348898008484E-23));
#15578=DIRECTION('center_axis',(-1.,-1.07791973573316E-23,-1.3010426069826E-18));
#15579=DIRECTION('ref_axis',(-1.3010426069826E-18,-1.40241950309628E-41,
1.));
#15580=DIRECTION('center_axis',(0.980042665160196,-3.01322847342843E-14,
0.198787259314322));
#15581=DIRECTION('ref_axis',(0.198787259314322,9.80607162696455E-12,-0.980042665160196));
#15582=DIRECTION('',(-1.,-1.07791973573316E-23,-1.30104260698261E-18));
#15583=DIRECTION('center_axis',(-1.,-1.07791973573316E-23,-1.3010426069826E-18));
#15584=DIRECTION('ref_axis',(1.3010426069826E-18,1.77064221811572E-15,-1.));
#15585=DIRECTION('center_axis',(5.42101086242751E-19,0.986391978972162,
0.164410656039629));
#15586=DIRECTION('ref_axis',(2.16840434497101E-18,-0.164410656039629,0.986391978972162));
#15587=DIRECTION('',(-0.196186965810001,-0.161215582689263,0.967222937250987));
#15588=DIRECTION('',(-1.,-1.07791973573316E-23,-1.30104260698261E-18));
#15589=DIRECTION('',(-2.168404344971E-18,0.164410656039629,-0.986391978972162));
#15590=DIRECTION('center_axis',(-1.,-1.07791973573316E-23,-1.3010426069826E-18));
#15591=DIRECTION('ref_axis',(-1.3010426069826E-18,-1.40241950309628E-41,
1.));
#15592=DIRECTION('center_axis',(-0.980042665160224,1.39583377813246E-13,
-0.198787259314183));
#15593=DIRECTION('ref_axis',(0.198787259314183,2.0130592482984E-11,-0.980042665160224));
#15594=DIRECTION('',(-1.,-1.07791973573316E-23,-1.30104260698261E-18));
#15595=DIRECTION('center_axis',(1.,1.07791973573316E-23,1.3010426069826E-18));
#15596=DIRECTION('ref_axis',(1.3010426069826E-18,1.40241950309628E-41,-1.));
#15597=DIRECTION('center_axis',(-1.3010426069826E-18,1.32348898008484E-23,
1.));
#15598=DIRECTION('ref_axis',(1.,1.07791973573316E-23,1.3010426069826E-18));
#15599=DIRECTION('',(-1.08050467514739E-23,-1.,-1.32348898008484E-23));
#15600=DIRECTION('',(-1.,-1.07791973573316E-23,-1.30104260698261E-18));
#15601=DIRECTION('',(1.08050467514739E-23,1.,1.32348898008484E-23));
#15602=DIRECTION('center_axis',(-1.08050467514739E-23,-1.,1.32348898008484E-23));
#15603=DIRECTION('ref_axis',(-3.46944695195361E-18,-1.32348898008484E-23,
-1.));
#15604=DIRECTION('',(0.198787259314375,-1.98523347012726E-23,-0.980042665160185));
#15605=DIRECTION('',(-1.,-1.07791973573316E-23,-1.30104260698261E-18));
#15606=DIRECTION('',(-3.46944695195361E-18,-1.32348898008484E-23,-1.));
#15607=DIRECTION('center_axis',(1.3010426069826E-18,-1.32348898008484E-23,
-1.));
#15608=DIRECTION('ref_axis',(-1.,-1.07791973573316E-23,-1.3010426069826E-18));
#15609=DIRECTION('',(1.08050467514739E-23,1.,1.32348898008484E-23));
#15610=DIRECTION('',(-1.08050467514739E-23,-1.,-1.32348898008484E-23));
#15611=DIRECTION('center_axis',(1.,1.07791973573316E-23,-3.46944695195361E-18));
#15612=DIRECTION('ref_axis',(-3.46944695195361E-18,-1.32348898008484E-23,
-1.));
#15613=DIRECTION('center_axis',(-0.980042665160186,-1.48892510259545E-23,
-0.198787259314375));
#15614=DIRECTION('ref_axis',(-0.198787259314375,1.98523347012726E-23,0.980042665160185));
#15615=DIRECTION('center_axis',(-0.980042665160186,5.16987882845642E-23,
-0.198787259314375));
#15616=DIRECTION('ref_axis',(-0.198787259314375,-1.98523347012727E-23,0.980042665160186));
#15617=DIRECTION('',(4.79764755280756E-23,-1.,1.32348898008484E-23));
#15618=DIRECTION('',(-0.198787259314375,-1.98523347012727E-23,0.980042665160185));
#15619=DIRECTION('',(-4.79764755280756E-23,1.,-1.32348898008484E-23));
#15620=DIRECTION('',(0.198787259314375,1.98523347012727E-23,-0.980042665160185));
#15621=DIRECTION('',(4.79764755280756E-23,-1.,1.32348898008484E-23));
#15622=DIRECTION('center_axis',(-0.980042665160192,-1.1109697417788E-14,
-0.198787259314345));
#15623=DIRECTION('ref_axis',(0.198787259314345,-8.89157906913263E-12,-0.980042665160192));
#15624=DIRECTION('',(-0.196186965810001,-0.161215582689263,0.967222937250987));
#15625=DIRECTION('center_axis',(0.980042665160184,-1.0212903229267E-14,
0.198787259314383));
#15626=DIRECTION('ref_axis',(0.198787259314383,-1.20235415482955E-11,-0.980042665160184));
#15627=DIRECTION('',(4.79764755280756E-23,-1.,1.32348898008484E-23));
#15628=DIRECTION('center_axis',(0.980042665160188,1.68386297044527E-14,
0.198787259314362));
#15629=DIRECTION('ref_axis',(0.198787259314362,5.91971428266698E-13,-0.980042665160188));
#15630=DIRECTION('',(0.196186965810001,-0.161215582689263,-0.967222937250987));
#15631=DIRECTION('center_axis',(-0.980042665160183,2.8030621177186E-14,
-0.198787259314389));
#15632=DIRECTION('ref_axis',(0.198787259314389,-8.39289157340378E-12,-0.980042665160183));
#15633=DIRECTION('center_axis',(0.389639990836698,6.61744490042423E-24,
-0.920967251068559));
#15634=DIRECTION('ref_axis',(-0.920967251068559,5.55244986176219E-23,-0.389639990836698));
#15635=DIRECTION('',(-0.920967251068559,6.70016296167952E-23,-0.389639990836698));
#15636=DIRECTION('',(-4.79764755280756E-23,1.,-1.32348898008484E-23));
#15637=DIRECTION('',(-0.920967251068559,6.70016296167952E-23,-0.389639990836698));
#15638=DIRECTION('center_axis',(4.79764755280756E-23,-1.,-3.63959469523332E-23));
#15639=DIRECTION('ref_axis',(-1.11022302462516E-16,3.63959469523332E-23,
-1.));
#15640=DIRECTION('',(0.198787259314375,1.32348898008484E-23,-0.980042665160185));
#15641=DIRECTION('',(-0.920967251068559,6.70016296167952E-23,-0.389639990836698));
#15642=DIRECTION('center_axis',(-0.389639990836698,-9.92616735063634E-24,
0.920967251068559));
#15643=DIRECTION('ref_axis',(0.920967251068559,-6.70016296167952E-23,0.389639990836698));
#15644=DIRECTION('',(4.79764755280756E-23,-1.,1.32348898008484E-23));
#15645=DIRECTION('',(-0.920967251068559,6.70016296167952E-23,-0.389639990836698));
#15646=DIRECTION('center_axis',(-0.920967251068559,6.70016296167952E-23,
-0.389639990836698));
#15647=DIRECTION('ref_axis',(-0.389639990836698,5.58402704648591E-37,0.920967251068559));
#15648=DIRECTION('center_axis',(-0.980042665160215,1.23232182126544E-13,
-0.198787259314232));
#15649=DIRECTION('ref_axis',(0.198787259314232,3.04736265298492E-11,-0.980042665160214));
#15650=DIRECTION('',(-0.920967251068559,6.70016296167952E-23,-0.389639990836698));
#15651=DIRECTION('center_axis',(-0.0640609665127368,0.986391978972162,0.151416829939196));
#15652=DIRECTION('ref_axis',(5.5015443345664E-17,-0.151728482244601,0.988422211241608));
#15653=DIRECTION('',(-0.196186965810001,-0.161215582689263,0.967222937250987));
#15654=DIRECTION('',(-0.920967251068559,6.70016296167952E-23,-0.389639990836698));
#15655=DIRECTION('center_axis',(-0.920967251068559,6.70016296167952E-23,
-0.389639990836698));
#15656=DIRECTION('ref_axis',(-0.389639990836698,1.72143967328141E-37,0.920967251068559));
#15657=DIRECTION('center_axis',(0.980042665160173,5.74370301447608E-14,
0.198787259314435));
#15658=DIRECTION('ref_axis',(0.198787259314435,-7.91172988590792E-12,-0.980042665160173));
#15659=DIRECTION('',(-0.920967251068559,6.70016296167952E-23,-0.389639990836698));
#15660=DIRECTION('center_axis',(-0.389639990836698,-9.92616735063634E-24,
0.920967251068559));
#15661=DIRECTION('ref_axis',(0.920967251068559,-6.70016296167952E-23,0.389639990836698));
#15662=DIRECTION('',(4.79764755280756E-23,-1.,1.32348898008484E-23));
#15663=DIRECTION('',(-0.920967251068559,6.70016296167952E-23,-0.389639990836698));
#15664=DIRECTION('center_axis',(-0.920967251068559,6.70016296167952E-23,
-0.389639990836698));
#15665=DIRECTION('ref_axis',(-0.389639990836698,1.72143967328141E-37,0.920967251068559));
#15666=DIRECTION('center_axis',(0.980042665160181,-1.32514529503713E-14,
0.198787259314395));
#15667=DIRECTION('ref_axis',(0.198787259314395,2.44975507155414E-12,-0.980042665160181));
#15668=DIRECTION('',(-0.920967251068559,6.70016296167952E-23,-0.389639990836698));
#15669=DIRECTION('center_axis',(-0.0640609665127368,-0.986391978972162,
0.151416829939196));
#15670=DIRECTION('ref_axis',(-5.50609226423701E-17,-0.151728482244601,-0.988422211241608));
#15671=DIRECTION('',(0.196186965810001,-0.161215582689263,-0.967222937250987));
#15672=DIRECTION('',(-0.920967251068559,6.70016296167952E-23,-0.389639990836698));
#15673=DIRECTION('center_axis',(-0.920967251068559,6.70016296167952E-23,
-0.389639990836698));
#15674=DIRECTION('ref_axis',(-0.389639990836698,5.58402704648591E-37,0.920967251068559));
#15675=DIRECTION('center_axis',(-0.980042665160197,-5.27568195326752E-14,
-0.198787259314317));
#15676=DIRECTION('ref_axis',(0.198787259314317,-5.60688280667672E-11,-0.980042665160197));
#15677=DIRECTION('',(-0.920967251068559,6.70016296167952E-23,-0.389639990836698));
#15678=DIRECTION('center_axis',(-0.389639990836698,-9.92616735063634E-24,
0.920967251068559));
#15679=DIRECTION('ref_axis',(0.920967251068559,-6.70016296167952E-23,0.389639990836698));
#15680=DIRECTION('',(4.79764755280756E-23,-1.,1.32348898008484E-23));
#15681=DIRECTION('',(-0.920967251068559,6.70016296167952E-23,-0.389639990836698));
#15682=DIRECTION('center_axis',(-4.79764755280756E-23,1.,3.63959469523332E-23));
#15683=DIRECTION('ref_axis',(1.11022302462516E-16,-3.63959469523332E-23,
1.));
#15684=DIRECTION('',(-0.198787259314375,-1.32348898008484E-23,0.980042665160185));
#15685=DIRECTION('center_axis',(-0.980042665160186,4.30133918527574E-23,
-0.198787259314375));
#15686=DIRECTION('ref_axis',(-0.198787259314375,-1.32348898008484E-23,0.980042665160185));
#15687=DIRECTION('center_axis',(1.28626585251996E-22,-1.,7.63278329429795E-17));
#15688=DIRECTION('ref_axis',(2.64697796016969E-23,-7.63278329429795E-17,
-1.));
#15689=DIRECTION('',(1.02125158911203E-14,-1.38777878078145E-17,-1.));
#15690=DIRECTION('',(1.,-1.48065329646992E-22,-3.97046694025453E-23));
#15691=DIRECTION('center_axis',(1.28626585251996E-22,-1.,4.85722573273505E-17));
#15692=DIRECTION('ref_axis',(-3.57010491314168E-39,-4.85722573273505E-17,
-1.));
#15693=DIRECTION('',(0.164410656039619,6.93889390390723E-18,0.986391978972164));
#15694=DIRECTION('center_axis',(-1.28626585251996E-22,1.,-4.85722573273505E-17));
#15695=DIRECTION('ref_axis',(-3.57010491314211E-39,-4.85722573273506E-17,
-1.));
#15696=DIRECTION('',(1.,-1.9935052762528E-22,1.0378694093902E-14));
#15697=DIRECTION('center_axis',(-1.28626585251996E-22,1.,-4.85722573273505E-17));
#15698=DIRECTION('ref_axis',(3.57010491314192E-39,4.85722573273505E-17,
1.));
#15699=DIRECTION('',(0.16441065603964,-2.77555756156289E-17,-0.986391978972161));
#15700=DIRECTION('center_axis',(1.28626585251996E-22,-1.,4.85722573273505E-17));
#15701=DIRECTION('ref_axis',(3.57010491314168E-39,4.85722573273505E-17,
1.));
#15702=DIRECTION('',(1.,-1.48065329646992E-22,-3.97046694025453E-23));
#15703=DIRECTION('',(-1.02125158911203E-14,1.38777878078145E-17,1.));
#15704=DIRECTION('',(-1.,1.72467157717306E-22,-1.0198899135044E-14));
#15705=DIRECTION('center_axis',(1.0198899135044E-14,-1.38777878078145E-17,
-1.));
#15706=DIRECTION('ref_axis',(-1.,1.72467157717306E-22,-1.0198899135044E-14));
#15707=DIRECTION('',(-1.23249911270401E-22,1.,1.38777878078144E-17));
#15708=DIRECTION('',(-1.,-1.00447013890157E-14,-1.01988991218091E-14));
#15709=DIRECTION('',(-1.23249911270401E-22,1.,1.38777878078144E-17));
#15710=DIRECTION('center_axis',(-1.,1.44343016890503E-22,-1.02125158911203E-14));
#15711=DIRECTION('ref_axis',(-1.02125158911203E-14,1.38777878078145E-17,
1.));
#15712=DIRECTION('',(-1.23249911270401E-22,1.,1.38777878078144E-17));
#15713=DIRECTION('',(-7.22133935627488E-15,0.707106781186548,0.707106781186547));
#15714=DIRECTION('center_axis',(3.97046694025453E-23,1.38777878078145E-17,
1.));
#15715=DIRECTION('ref_axis',(1.,-1.48065329646992E-22,-3.97046694025453E-23));
#15716=DIRECTION('',(-1.23249911270401E-22,1.,1.38777878078144E-17));
#15717=DIRECTION('',(1.,-1.54197836190994E-16,-3.97046694025453E-23));
#15718=DIRECTION('center_axis',(-1.23249911270401E-22,1.,1.38777878078144E-17));
#15719=DIRECTION('ref_axis',(3.42087223188502E-39,-1.38777878078144E-17,
1.));
#15720=DIRECTION('',(-1.23249911270401E-22,1.,1.38777878078144E-17));
#15721=DIRECTION('center_axis',(-2.13533570892991E-15,-0.70710678118654,
0.707106781186555));
#15722=DIRECTION('ref_axis',(-5.92260635202438E-13,-0.707106781186555,-0.70710678118654));
#15723=DIRECTION('center_axis',(0.986391978972161,4.33680868994202E-18,
0.16441065603964));
#15724=DIRECTION('ref_axis',(0.16441065603964,-2.77555756156289E-17,-0.986391978972161));
#15725=DIRECTION('',(-1.23249911270401E-22,1.,1.38777878078144E-17));
#15726=DIRECTION('',(0.117049568370797,-0.702246181386631,-0.702246181386631));
#15727=DIRECTION('center_axis',(-1.23249911270401E-22,1.,1.38777878078144E-17));
#15728=DIRECTION('ref_axis',(3.42087223188512E-39,-1.38777878078144E-17,
1.));
#15729=DIRECTION('',(-1.23249911270401E-22,1.,1.38777878078144E-17));
#15730=DIRECTION('center_axis',(5.7517460173195E-15,0.70710678118654,-0.707106781186555));
#15731=DIRECTION('ref_axis',(1.26621527472326E-13,0.707106781186555,0.70710678118654));
#15732=DIRECTION('center_axis',(-1.0378694093902E-14,1.38777878078145E-17,
1.));
#15733=DIRECTION('ref_axis',(1.,-1.9935052762528E-22,1.0378694093902E-14));
#15734=DIRECTION('',(-1.23249911270401E-22,1.,1.38777878078144E-17));
#15735=DIRECTION('',(1.,1.02244962936934E-14,1.0378694093902E-14));
#15736=DIRECTION('center_axis',(-1.23249911270401E-22,1.,1.38777878078144E-17));
#15737=DIRECTION('ref_axis',(3.42087223188522E-39,-1.38777878078144E-17,
1.));
#15738=DIRECTION('',(-1.23249911270401E-22,1.,1.38777878078144E-17));
#15739=DIRECTION('center_axis',(-1.20786666363705E-14,0.70710678118656,
-0.707106781186535));
#15740=DIRECTION('ref_axis',(5.92625417861852E-14,0.707106781186535,0.70710678118656));
#15741=DIRECTION('center_axis',(-0.986391978972164,6.93889390390723E-18,
0.164410656039619));
#15742=DIRECTION('ref_axis',(0.164410656039619,2.77555756156289E-17,0.986391978972164));
#15743=DIRECTION('',(-1.23249911270401E-22,1.,1.38777878078144E-17));
#15744=DIRECTION('',(0.117049568370782,0.702246181386633,0.702246181386632));
#15745=DIRECTION('center_axis',(-1.23249911270401E-22,1.,1.38777878078144E-17));
#15746=DIRECTION('ref_axis',(3.42087223188502E-39,-1.38777878078144E-17,
1.));
#15747=DIRECTION('',(-1.23249911270401E-22,1.,1.38777878078144E-17));
#15748=DIRECTION('center_axis',(-2.31004499420576E-14,-0.707106781186537,
0.707106781186558));
#15749=DIRECTION('ref_axis',(2.54103796788768E-13,-0.707106781186558,-0.707106781186537));
#15750=DIRECTION('center_axis',(3.97046694025453E-23,1.38777878078145E-17,
1.));
#15751=DIRECTION('ref_axis',(1.,-1.48065329646992E-22,-3.97046694025453E-23));
#15752=DIRECTION('',(-1.23249911270401E-22,1.,1.38777878078144E-17));
#15753=DIRECTION('',(1.,-1.54197836190994E-16,-3.97046694025453E-23));
#15754=DIRECTION('center_axis',(1.,-1.44343016890503E-22,1.02125158911203E-14));
#15755=DIRECTION('ref_axis',(1.02125158911203E-14,-1.38777878078145E-17,
-1.));
#15756=DIRECTION('',(7.22133935627488E-15,-0.707106781186548,-0.707106781186547));
#15757=DIRECTION('center_axis',(-1.09034144081742E-16,-0.707106781186547,
0.707106781186548));
#15758=DIRECTION('ref_axis',(1.19114008210604E-22,-0.707106781186548,-0.707106781186547));
#15759=DIRECTION('center_axis',(1.2516276642837E-22,1.,7.63278329429795E-17));
#15760=DIRECTION('ref_axis',(-3.08395300977893E-16,-7.63278329429795E-17,
1.));
#15761=DIRECTION('',(9.90412056201823E-15,-1.38777878078144E-16,1.));
#15762=DIRECTION('',(-1.,-5.28361616268246E-23,9.89050390189491E-15));
#15763=DIRECTION('',(-9.90412056201823E-15,1.38777878078144E-16,-1.));
#15764=DIRECTION('',(1.,6.97416653958771E-23,3.08395271199391E-16));
#15765=DIRECTION('center_axis',(1.2516276643693E-22,1.,4.85722573273506E-17));
#15766=DIRECTION('ref_axis',(-3.47396462810159E-39,4.85722573273506E-17,
-1.));
#15767=DIRECTION('',(0.16441065603964,-1.2490009027033E-16,0.986391978972161));
#15768=DIRECTION('center_axis',(-1.2516276643693E-22,-1.,-4.85722573273506E-17));
#15769=DIRECTION('ref_axis',(-3.47396462810152E-39,4.85722573273506E-17,
-1.));
#15770=DIRECTION('',(1.,1.18907213054498E-23,-1.00702988590986E-14));
#15771=DIRECTION('center_axis',(-1.2516276643693E-22,-1.,-4.85722573273506E-17));
#15772=DIRECTION('ref_axis',(3.47396462810149E-39,-4.85722573273506E-17,
1.));
#15773=DIRECTION('',(0.164410656039619,1.04083408558608E-16,-0.986391978972164));
#15774=DIRECTION('center_axis',(1.2516276643693E-22,1.,4.85722573273506E-17));
#15775=DIRECTION('ref_axis',(3.47396462810128E-39,-4.85722573273506E-17,
1.));
#15776=DIRECTION('',(1.,6.97416653958771E-23,3.08395271199391E-16));
#15777=DIRECTION('center_axis',(9.89050390189491E-15,-1.38777878078144E-17,
1.));
#15778=DIRECTION('ref_axis',(1.,5.28361616268246E-23,-9.89050390189491E-15));
#15779=DIRECTION('',(-1.26041645837768E-22,-1.,1.38777878078145E-17));
#15780=DIRECTION('',(1.,1.00447015947769E-14,-9.89050390024055E-15));
#15781=DIRECTION('',(-1.26041645837768E-22,-1.,1.38777878078145E-17));
#15782=DIRECTION('center_axis',(-1.,2.37814426108995E-23,9.90412057029004E-15));
#15783=DIRECTION('ref_axis',(9.90412057029004E-15,-1.38777878078144E-17,
1.));
#15784=DIRECTION('',(7.00327079679616E-15,-0.707106781186548,0.707106781186548));
#15785=DIRECTION('',(-1.26041645837768E-22,-1.,1.38777878078145E-17));
#15786=DIRECTION('center_axis',(3.08395271199391E-16,1.38777878078144E-17,
-1.));
#15787=DIRECTION('ref_axis',(-1.,-6.97416653958771E-23,-3.08395271199391E-16));
#15788=DIRECTION('',(-1.,1.54197564307067E-16,-3.0839526954503E-16));
#15789=DIRECTION('',(-1.26041645837768E-22,-1.,1.38777878078145E-17));
#15790=DIRECTION('center_axis',(-1.26041645837768E-22,-1.,1.38777878078145E-17));
#15791=DIRECTION('ref_axis',(-1.74917921588424E-39,-1.38777878078145E-17,
-1.));
#15792=DIRECTION('center_axis',(-1.54326535327199E-14,-0.707106781186548,
-0.707106781186547));
#15793=DIRECTION('ref_axis',(-1.3938976131661E-12,0.707106781186547,-0.707106781186548));
#15794=DIRECTION('',(-1.26041645837768E-22,-1.,1.38777878078145E-17));
#15795=DIRECTION('center_axis',(0.986391978972161,-2.60208521396521E-18,
-0.16441065603964));
#15796=DIRECTION('ref_axis',(-0.16441065603964,2.83749245036362E-35,-0.986391978972161));
#15797=DIRECTION('',(-0.117049568370797,0.702246181386631,-0.702246181386631));
#15798=DIRECTION('',(-1.26041645837768E-22,-1.,1.38777878078145E-17));
#15799=DIRECTION('center_axis',(-1.26041645837768E-22,-1.,1.38777878078145E-17));
#15800=DIRECTION('ref_axis',(-1.74917921588424E-39,-1.38777878078144E-17,
-1.));
#15801=DIRECTION('center_axis',(1.4379365043299E-15,0.707106781186542,0.707106781186553));
#15802=DIRECTION('ref_axis',(1.34200807773731E-12,-0.707106781186553,0.707106781186542));
#15803=DIRECTION('',(-1.26041645837768E-22,-1.,1.38777878078145E-17));
#15804=DIRECTION('center_axis',(-1.00702988590986E-14,1.38777878078144E-17,
-1.));
#15805=DIRECTION('ref_axis',(-1.,-1.18907213054498E-23,1.00702988590986E-14));
#15806=DIRECTION('',(-1.,-1.02244964855993E-14,1.00702988557898E-14));
#15807=DIRECTION('',(-1.26041645837768E-22,-1.,1.38777878078145E-17));
#15808=DIRECTION('center_axis',(-1.26041645837768E-22,-1.,1.38777878078145E-17));
#15809=DIRECTION('ref_axis',(-1.74917921588424E-39,-1.38777878078145E-17,
-1.));
#15810=DIRECTION('center_axis',(1.29414285389683E-14,0.707106781186545,
0.70710678118655));
#15811=DIRECTION('ref_axis',(1.69540060192356E-13,-0.70710678118655,0.707106781186545));
#15812=DIRECTION('',(-1.26041645837768E-22,-1.,1.38777878078145E-17));
#15813=DIRECTION('center_axis',(-0.986391978972164,2.60208521396522E-18,
-0.164410656039619));
#15814=DIRECTION('ref_axis',(-0.164410656039619,2.08166817117217E-17,0.986391978972164));
#15815=DIRECTION('',(-0.117049568370783,-0.702246181386632,0.702246181386632));
#15816=DIRECTION('',(-1.26041645837768E-22,-1.,1.38777878078145E-17));
#15817=DIRECTION('center_axis',(-1.26041645837768E-22,-1.,1.38777878078145E-17));
#15818=DIRECTION('ref_axis',(-1.74917921588424E-39,-1.38777878078145E-17,
-1.));
#15819=DIRECTION('center_axis',(1.94121428084521E-14,-0.707106781186553,
-0.707106781186542));
#15820=DIRECTION('ref_axis',(6.99433665140334E-13,0.707106781186542,-0.707106781186553));
#15821=DIRECTION('',(-1.26041645837768E-22,-1.,1.38777878078145E-17));
#15822=DIRECTION('center_axis',(3.08395271199391E-16,1.38777878078144E-17,
-1.));
#15823=DIRECTION('ref_axis',(-1.,-6.97416653958771E-23,-3.08395271199391E-16));
#15824=DIRECTION('',(-1.,1.54197564307067E-16,-3.0839526954503E-16));
#15825=DIRECTION('',(-1.26041645837768E-22,-1.,1.38777878078145E-17));
#15826=DIRECTION('center_axis',(1.,-2.37814426108995E-23,-9.90412057029004E-15));
#15827=DIRECTION('ref_axis',(-9.90412057029004E-15,1.38777878078144E-17,
-1.));
#15828=DIRECTION('',(-7.00327079679616E-15,0.707106781186548,-0.707106781186548));
#15829=DIRECTION('center_axis',(1.09034183786412E-16,-0.707106781186548,
-0.707106781186547));
#15830=DIRECTION('ref_axis',(4.63221142954057E-23,0.707106781186547,-0.707106781186548));
#15831=DIRECTION('center_axis',(1.,-3.54987407349455E-30,-1.04916075827077E-14));
#15832=DIRECTION('ref_axis',(-1.04916075827077E-14,-9.86076131526265E-32,
-1.));
#15833=DIRECTION('',(1.04916075827077E-14,3.82856869892695E-16,1.));
#15834=DIRECTION('',(0.,-1.,3.46944695195361E-16));
#15835=DIRECTION('',(1.04916075827077E-14,3.82856869892695E-16,1.));
#15836=DIRECTION('',(0.,-1.,3.46944695195361E-16));
#15837=DIRECTION('center_axis',(0.,-3.46944695195361E-16,-1.));
#15838=DIRECTION('ref_axis',(0.,1.,-3.46944695195361E-16));
#15839=DIRECTION('',(1.,0.,0.));
#15840=DIRECTION('',(0.,-1.,3.46944695195361E-16));
#15841=DIRECTION('',(1.,0.,0.));
#15842=DIRECTION('center_axis',(0.,-1.,3.46944695195361E-16));
#15843=DIRECTION('ref_axis',(0.,-3.46944695195361E-16,-1.));
#15844=DIRECTION('center_axis',(4.93038065763132E-32,1.,-3.82856869892695E-16));
#15845=DIRECTION('ref_axis',(0.,3.82856869892695E-16,1.));
#15846=DIRECTION('',(0.,-1.,3.46944695195361E-16));
#15847=DIRECTION('center_axis',(4.93038065763132E-32,1.,-3.82856869892695E-16));
#15848=DIRECTION('ref_axis',(1.88763010596022E-47,3.82856869892695E-16,
1.));
#15849=DIRECTION('center_axis',(-1.,3.54987407349455E-30,1.06581410364015E-14));
#15850=DIRECTION('ref_axis',(1.06581410364015E-14,1.97215226305253E-31,
1.));
#15851=DIRECTION('',(-1.06581410364015E-14,-3.82856869892696E-16,-1.));
#15852=DIRECTION('',(0.,-1.,3.46944695195361E-16));
#15853=DIRECTION('',(-1.06581410364015E-14,-3.82856869892696E-16,-1.));
#15854=DIRECTION('center_axis',(0.,-1.,3.46944695195361E-16));
#15855=DIRECTION('ref_axis',(0.,-3.46944695195361E-16,-1.));
#15856=DIRECTION('center_axis',(-4.93038065763132E-32,-1.,3.82856869892695E-16));
#15857=DIRECTION('ref_axis',(-9.72346137165803E-63,-3.82856869892695E-16,
-1.));
#15858=DIRECTION('',(0.,-1.,3.46944695195361E-16));
#15859=DIRECTION('center_axis',(-4.93038065763132E-32,-1.,3.82856869892695E-16));
#15860=DIRECTION('ref_axis',(-1.88763010596022E-47,-3.82856869892695E-16,
-1.));
#15861=DIRECTION('center_axis',(-1.16018306073329E-14,-3.46944695195361E-16,
-1.));
#15862=DIRECTION('ref_axis',(-1.,0.,1.16018306073329E-14));
#15863=DIRECTION('',(1.,-4.73316543132607E-30,-1.16018306073329E-14));
#15864=DIRECTION('',(0.,-1.,3.46944695195361E-16));
#15865=DIRECTION('',(1.,-4.73316543132607E-30,-1.16018306073329E-14));
#15866=DIRECTION('center_axis',(0.,-1.,3.46944695195361E-16));
#15867=DIRECTION('ref_axis',(0.,-3.46944695195361E-16,-1.));
#15868=DIRECTION('center_axis',(4.93038065763132E-32,1.,-3.82856869892695E-16));
#15869=DIRECTION('ref_axis',(-2.43086534291451E-62,-3.82856869892695E-16,
-1.));
#15870=DIRECTION('',(0.,-1.,3.46944695195361E-16));
#15871=DIRECTION('center_axis',(4.93038065763132E-32,1.,-3.82856869892695E-16));
#15872=DIRECTION('ref_axis',(-1.88763010596022E-47,-3.82856869892695E-16,
-1.));
#15873=DIRECTION('center_axis',(-1.,0.,0.));
#15874=DIRECTION('ref_axis',(0.,9.86076131526265E-32,1.));
#15875=DIRECTION('',(0.,-3.82856869891308E-16,-1.));
#15876=DIRECTION('',(0.,-1.,3.46944695195361E-16));
#15877=DIRECTION('',(0.,-3.82856869891308E-16,-1.));
#15878=DIRECTION('center_axis',(1.0991207943789E-14,3.46944695195361E-16,
1.));
#15879=DIRECTION('ref_axis',(1.,0.,-1.0991207943789E-14));
#15880=DIRECTION('',(-1.,3.94430452610506E-30,1.0991207943789E-14));
#15881=DIRECTION('',(-1.,3.94430452610506E-30,1.0991207943789E-14));
#15882=DIRECTION('center_axis',(-4.93038065763132E-32,-1.,3.82856869892695E-16));
#15883=DIRECTION('ref_axis',(0.,-3.82856869892695E-16,-1.));
#15884=DIRECTION('center_axis',(-4.93038065763132E-32,-1.,3.82856869892695E-16));
#15885=DIRECTION('ref_axis',(0.,-3.82856869892695E-16,-1.));
#15886=DIRECTION('center_axis',(-1.,-6.85322911410754E-30,-1.02140518265514E-14));
#15887=DIRECTION('ref_axis',(-1.02140518265514E-14,0.,1.));
#15888=DIRECTION('',(-1.02140518265514E-14,6.57977215693388E-16,1.));
#15889=DIRECTION('',(-1.75644810928116E-31,1.,-6.93889390390723E-16));
#15890=DIRECTION('',(-1.02140518265514E-14,6.57977215693388E-16,1.));
#15891=DIRECTION('',(-1.75644810928116E-31,1.,-6.93889390390723E-16));
#15892=DIRECTION('center_axis',(-1.11022302462516E-16,-6.93889390390723E-16,
-1.));
#15893=DIRECTION('ref_axis',(-1.75644810928116E-31,1.,-6.93889390390723E-16));
#15894=DIRECTION('',(-1.,-1.22464679914735E-16,1.11022302462516E-16));
#15895=DIRECTION('',(-1.75644810928116E-31,1.,-6.93889390390723E-16));
#15896=DIRECTION('',(-1.,-1.22464679914735E-16,1.11022302462516E-16));
#15897=DIRECTION('center_axis',(-1.75644810928116E-31,1.,-6.93889390390723E-16));
#15898=DIRECTION('ref_axis',(7.77876909732643E-62,6.93889390390723E-16,
1.));
#15899=DIRECTION('center_axis',(1.22464679914736E-16,-1.,6.57977215693389E-16));
#15900=DIRECTION('ref_axis',(-8.05789691110799E-32,6.57977215693389E-16,
1.));
#15901=DIRECTION('',(-1.75644810928116E-31,1.,-6.93889390390723E-16));
#15902=DIRECTION('center_axis',(1.22464679914736E-16,-1.,6.57977215693389E-16));
#15903=DIRECTION('ref_axis',(6.07126862973252E-47,6.57977215693389E-16,
1.));
#15904=DIRECTION('center_axis',(1.,7.09974814698911E-30,1.0547118733939E-14));
#15905=DIRECTION('ref_axis',(1.0547118733939E-14,1.4791141972894E-31,-1.));
#15906=DIRECTION('',(1.0547118733939E-14,-6.57977215693387E-16,-1.));
#15907=DIRECTION('',(-1.75644810928116E-31,1.,-6.93889390390723E-16));
#15908=DIRECTION('',(1.0547118733939E-14,-6.57977215693387E-16,-1.));
#15909=DIRECTION('center_axis',(-1.75644810928116E-31,1.,-6.93889390390723E-16));
#15910=DIRECTION('ref_axis',(0.,6.93889390390723E-16,1.));
#15911=DIRECTION('center_axis',(-1.22464679914736E-16,1.,-6.57977215693389E-16));
#15912=DIRECTION('ref_axis',(8.05789691110799E-32,-6.57977215693389E-16,
-1.));
#15913=DIRECTION('',(-1.75644810928116E-31,1.,-6.93889390390723E-16));
#15914=DIRECTION('center_axis',(-1.22464679914736E-16,1.,-6.57977215693389E-16));
#15915=DIRECTION('ref_axis',(4.9731792179006E-48,-6.57977215693389E-16,
-1.));
#15916=DIRECTION('center_axis',(1.14908083048704E-14,-6.93889390390723E-16,
-1.));
#15917=DIRECTION('ref_axis',(-1.,1.4791141972894E-31,-1.14908083048704E-14));
#15918=DIRECTION('',(-1.,-1.22464679914743E-16,-1.14908083048704E-14));
#15919=DIRECTION('',(-1.75644810928116E-31,1.,-6.93889390390723E-16));
#15920=DIRECTION('',(-1.,-1.22464679914743E-16,-1.14908083048704E-14));
#15921=DIRECTION('center_axis',(-1.75644810928116E-31,1.,-6.93889390390723E-16));
#15922=DIRECTION('ref_axis',(-7.77876909732643E-62,6.93889390390723E-16,
1.));
#15923=DIRECTION('center_axis',(1.22464679914736E-16,-1.,6.57977215693389E-16));
#15924=DIRECTION('ref_axis',(8.05789691110799E-32,-6.57977215693389E-16,
-1.));
#15925=DIRECTION('',(-1.75644810928116E-31,1.,-6.93889390390723E-16));
#15926=DIRECTION('center_axis',(1.22464679914736E-16,-1.,6.57977215693389E-16));
#15927=DIRECTION('ref_axis',(1.25397265995815E-46,-6.57977215693389E-16,
-1.));
#15928=DIRECTION('center_axis',(1.,-2.95822839457879E-31,-1.11022302462516E-16));
#15929=DIRECTION('ref_axis',(-1.11022302462516E-16,0.,-1.));
#15930=DIRECTION('',(-1.11022302462516E-16,-6.57977215694776E-16,-1.));
#15931=DIRECTION('',(-1.75644810928116E-31,1.,-6.93889390390723E-16));
#15932=DIRECTION('',(-1.11022302462516E-16,-6.57977215694776E-16,-1.));
#15933=DIRECTION('center_axis',(-1.07136521876328E-14,6.93889390390723E-16,
1.));
#15934=DIRECTION('ref_axis',(1.,-3.45126646034193E-31,1.07136521876328E-14));
#15935=DIRECTION('',(1.,1.22464679914742E-16,1.07136521876328E-14));
#15936=DIRECTION('',(1.,1.22464679914742E-16,1.07136521876328E-14));
#15937=DIRECTION('center_axis',(-1.22464679914736E-16,1.,-6.57977215693389E-16));
#15938=DIRECTION('ref_axis',(-1.11022302462516E-16,-6.57977215693389E-16,
-1.));
#15939=DIRECTION('center_axis',(-1.22464679914736E-16,1.,-6.57977215693389E-16));
#15940=DIRECTION('ref_axis',(-1.11022302462516E-16,-6.57977215693389E-16,
-1.));
#15941=DIRECTION('center_axis',(1.,-3.6253356482683E-30,1.04493185757658E-14));
#15942=DIRECTION('ref_axis',(-1.04493185757658E-14,0.,1.));
#15943=DIRECTION('',(1.04493185757658E-14,3.82856869892695E-16,-1.));
#15944=DIRECTION('',(0.,-1.,-3.46944695195361E-16));
#15945=DIRECTION('',(1.04493185757658E-14,3.82856869892695E-16,-1.));
#15946=DIRECTION('',(0.,-1.,-3.46944695195361E-16));
#15947=DIRECTION('center_axis',(0.,-3.46944695195361E-16,1.));
#15948=DIRECTION('ref_axis',(0.,1.,3.46944695195361E-16));
#15949=DIRECTION('',(1.,0.,0.));
#15950=DIRECTION('',(1.,0.,0.));
#15951=DIRECTION('',(0.,-1.,-3.46944695195361E-16));
#15952=DIRECTION('center_axis',(0.,-1.,-3.46944695195361E-16));
#15953=DIRECTION('ref_axis',(0.,-3.46944695195361E-16,1.));
#15954=DIRECTION('center_axis',(0.,-1.,-3.82856869892695E-16));
#15955=DIRECTION('ref_axis',(0.,3.82856869892695E-16,-1.));
#15956=DIRECTION('center_axis',(0.,-1.,-3.82856869892695E-16));
#15957=DIRECTION('ref_axis',(0.,3.82856869892695E-16,-1.));
#15958=DIRECTION('',(0.,-1.,-3.46944695195361E-16));
#15959=DIRECTION('center_axis',(-1.,3.70563421514164E-30,-1.06807634371093E-14));
#15960=DIRECTION('ref_axis',(1.06807634371093E-14,0.,-1.));
#15961=DIRECTION('',(-1.06807634371093E-14,-3.82856869892695E-16,1.));
#15962=DIRECTION('',(-1.06807634371093E-14,-3.82856869892695E-16,1.));
#15963=DIRECTION('',(0.,-1.,-3.46944695195361E-16));
#15964=DIRECTION('center_axis',(0.,-1.,-3.46944695195361E-16));
#15965=DIRECTION('ref_axis',(0.,-3.46944695195361E-16,1.));
#15966=DIRECTION('center_axis',(0.,1.,3.82856869892695E-16));
#15967=DIRECTION('ref_axis',(0.,-3.82856869892695E-16,1.));
#15968=DIRECTION('center_axis',(0.,1.,3.82856869892695E-16));
#15969=DIRECTION('ref_axis',(0.,-3.82856869892695E-16,1.));
#15970=DIRECTION('',(0.,-1.,-3.46944695195361E-16));
#15971=DIRECTION('center_axis',(-1.16517419313919E-14,-3.46944695195361E-16,
1.));
#15972=DIRECTION('ref_axis',(-1.,-1.09476442525376E-46,-1.16517419313919E-14));
#15973=DIRECTION('',(1.,-4.5545613262468E-30,1.16517419313919E-14));
#15974=DIRECTION('',(1.,-4.5545613262468E-30,1.16517419313919E-14));
#15975=DIRECTION('',(0.,-1.,-3.46944695195361E-16));
#15976=DIRECTION('center_axis',(0.,-1.,-3.46944695195361E-16));
#15977=DIRECTION('ref_axis',(0.,-3.46944695195361E-16,1.));
#15978=DIRECTION('center_axis',(0.,-1.,-3.82856869892695E-16));
#15979=DIRECTION('ref_axis',(0.,-3.82856869892695E-16,1.));
#15980=DIRECTION('center_axis',(0.,-1.,-3.82856869892695E-16));
#15981=DIRECTION('ref_axis',(0.,-3.82856869892695E-16,1.));
#15982=DIRECTION('',(0.,-1.,-3.46944695195361E-16));
#15983=DIRECTION('center_axis',(-1.,0.,0.));
#15984=DIRECTION('ref_axis',(0.,0.,-1.));
#15985=DIRECTION('',(0.,-3.82856869891308E-16,1.));
#15986=DIRECTION('',(0.,-3.82856869891308E-16,1.));
#15987=DIRECTION('',(0.,-1.,-3.46944695195361E-16));
#15988=DIRECTION('center_axis',(1.09273919746571E-14,3.46944695195361E-16,
-1.));
#15989=DIRECTION('ref_axis',(1.,-3.28429327576129E-46,1.09273919746571E-14));
#15990=DIRECTION('',(-1.,4.01021285003471E-30,-1.09273919746571E-14));
#15991=DIRECTION('',(-1.,4.01021285003471E-30,-1.09273919746571E-14));
#15992=DIRECTION('center_axis',(0.,-1.,-3.82856869892695E-16));
#15993=DIRECTION('ref_axis',(0.,-3.82856869892695E-16,1.));
#15994=DIRECTION('center_axis',(0.,-1.,-3.82856869892695E-16));
#15995=DIRECTION('ref_axis',(0.,-3.82856869892695E-16,1.));
#15996=DIRECTION('center_axis',(-1.,-7.10622655070755E-30,1.02411517586486E-14));
#15997=DIRECTION('ref_axis',(-1.02411517586486E-14,0.,-1.));
#15998=DIRECTION('',(-1.02411517586486E-14,6.57977215693388E-16,-1.));
#15999=DIRECTION('',(0.,1.,6.93889390390723E-16));
#16000=DIRECTION('',(-1.02411517586486E-14,6.57977215693388E-16,-1.));
#16001=DIRECTION('',(0.,1.,6.93889390390723E-16));
#16002=DIRECTION('center_axis',(-2.08166817117217E-16,-6.93889390390723E-16,
1.));
#16003=DIRECTION('ref_axis',(0.,1.,6.93889390390723E-16));
#16004=DIRECTION('',(-1.,-1.22464679914735E-16,-2.08166817117217E-16));
#16005=DIRECTION('',(-1.,-1.22464679914735E-16,-2.08166817117217E-16));
#16006=DIRECTION('',(0.,1.,6.93889390390723E-16));
#16007=DIRECTION('center_axis',(0.,1.,6.93889390390723E-16));
#16008=DIRECTION('ref_axis',(0.,6.93889390390723E-16,-1.));
#16009=DIRECTION('center_axis',(-1.22464679914735E-16,1.,6.57977215693389E-16));
#16010=DIRECTION('ref_axis',(-8.05789691110797E-32,6.57977215693389E-16,
-1.));
#16011=DIRECTION('center_axis',(-1.22464679914735E-16,1.,6.57977215693389E-16));
#16012=DIRECTION('ref_axis',(7.11800305454381E-47,6.57977215693389E-16,
-1.));
#16013=DIRECTION('',(0.,1.,6.93889390390723E-16));
#16014=DIRECTION('center_axis',(1.,7.26682368445424E-30,-1.04725966199921E-14));
#16015=DIRECTION('ref_axis',(1.04725966199921E-14,0.,1.));
#16016=DIRECTION('',(1.04725966199921E-14,-6.57977215693388E-16,1.));
#16017=DIRECTION('',(1.04725966199921E-14,-6.57977215693388E-16,1.));
#16018=DIRECTION('',(0.,1.,6.93889390390723E-16));
#16019=DIRECTION('center_axis',(0.,1.,6.93889390390723E-16));
#16020=DIRECTION('ref_axis',(0.,6.93889390390723E-16,-1.));
#16021=DIRECTION('center_axis',(1.22464679914735E-16,-1.,-6.57977215693389E-16));
#16022=DIRECTION('ref_axis',(8.05789691110797E-32,-6.57977215693389E-16,
1.));
#16023=DIRECTION('center_axis',(1.22464679914735E-16,-1.,-6.57977215693389E-16));
#16024=DIRECTION('ref_axis',(-1.64418092827499E-47,-6.57977215693389E-16,
1.));
#16025=DIRECTION('',(0.,1.,6.93889390390723E-16));
#16026=DIRECTION('center_axis',(1.14435751142747E-14,-6.93889390390723E-16,
1.));
#16027=DIRECTION('ref_axis',(-1.,-8.75811540203011E-47,1.14435751142747E-14));
#16028=DIRECTION('',(-1.,-1.22464679914743E-16,1.14435751142747E-14));
#16029=DIRECTION('',(-1.,-1.22464679914743E-16,1.14435751142747E-14));
#16030=DIRECTION('',(0.,1.,6.93889390390723E-16));
#16031=DIRECTION('center_axis',(0.,1.,6.93889390390723E-16));
#16032=DIRECTION('ref_axis',(0.,6.93889390390723E-16,-1.));
#16033=DIRECTION('center_axis',(-1.22464679914735E-16,1.,6.57977215693389E-16));
#16034=DIRECTION('ref_axis',(8.05789691110797E-32,-6.57977215693389E-16,
1.));
#16035=DIRECTION('center_axis',(-1.22464679914735E-16,1.,6.57977215693389E-16));
#16036=DIRECTION('ref_axis',(1.03982277495164E-46,-6.57977215693389E-16,
1.));
#16037=DIRECTION('',(0.,1.,6.93889390390723E-16));
#16038=DIRECTION('center_axis',(1.,-1.44444745829043E-31,2.08166817117217E-16));
#16039=DIRECTION('ref_axis',(-2.08166817117217E-16,0.,1.));
#16040=DIRECTION('',(-2.08166817117217E-16,-6.57977215694776E-16,1.));
#16041=DIRECTION('',(-2.08166817117217E-16,-6.57977215694776E-16,1.));
#16042=DIRECTION('',(0.,1.,6.93889390390723E-16));
#16043=DIRECTION('center_axis',(-1.07192251575398E-14,6.93889390390723E-16,
-1.));
#16044=DIRECTION('ref_axis',(1.,6.56858655152258E-46,-1.07192251575398E-14));
#16045=DIRECTION('',(1.,1.22464679914743E-16,-1.07192251575398E-14));
#16046=DIRECTION('',(1.,1.22464679914743E-16,-1.07192251575398E-14));
#16047=DIRECTION('center_axis',(-1.22464679914735E-16,1.,6.57977215693389E-16));
#16048=DIRECTION('ref_axis',(-2.08166817117217E-16,-6.57977215693389E-16,
1.));
#16049=DIRECTION('center_axis',(-1.22464679914735E-16,1.,6.57977215693389E-16));
#16050=DIRECTION('ref_axis',(-2.08166817117217E-16,-6.57977215693389E-16,
1.));
#16051=DIRECTION('center_axis',(3.46944695195361E-17,1.,-1.14491749414469E-16));
#16052=DIRECTION('ref_axis',(2.13821176807408E-50,1.14491749414469E-16,
1.));
#16053=DIRECTION('',(1.09356967925578E-14,-5.89805981832114E-17,-1.));
#16054=DIRECTION('',(1.,4.77048955893622E-17,-5.55111512312578E-17));
#16055=DIRECTION('center_axis',(-3.46944695195361E-17,-1.,2.16840434497101E-17));
#16056=DIRECTION('ref_axis',(3.21991412577252E-33,-2.16840434497101E-17,
-1.));
#16057=DIRECTION('',(-7.71605002114484E-15,6.33174068731535E-17,1.));
#16058=DIRECTION('center_axis',(3.46944695195361E-17,1.,-2.16840434497101E-17));
#16059=DIRECTION('ref_axis',(-3.21991412577236E-33,2.16840434497101E-17,
1.));
#16060=DIRECTION('',(1.,5.29090660172926E-17,1.16018306073329E-14));
#16061=DIRECTION('center_axis',(-3.46944695195361E-17,-1.,2.16840434497101E-17));
#16062=DIRECTION('ref_axis',(-3.2199141257724E-33,2.16840434497101E-17,
1.));
#16063=DIRECTION('',(0.,5.20417042793042E-17,1.));
#16064=DIRECTION('',(-1.,-4.77048955893622E-17,-1.03805852802452E-14));
#16065=DIRECTION('center_axis',(1.03805852802452E-14,-5.72458747072346E-17,
-1.));
#16066=DIRECTION('ref_axis',(-1.,-4.77048955893622E-17,-1.03805852802452E-14));
#16067=DIRECTION('',(4.59701721133853E-17,1.,4.16333634234433E-17));
#16068=DIRECTION('',(-1.,-1.04308922610485E-14,-1.04360964314765E-14));
#16069=DIRECTION('',(4.59701721133853E-17,1.,4.16333634234433E-17));
#16070=DIRECTION('center_axis',(-1.,-4.77048955893622E-17,2.48264406893667E-33));
#16071=DIRECTION('ref_axis',(0.,5.20417042793042E-17,1.));
#16072=DIRECTION('',(4.59701721133853E-17,1.,4.16333634234433E-17));
#16073=DIRECTION('',(-2.77555756156289E-16,0.707106781186548,0.707106781186547));
#16074=DIRECTION('center_axis',(4.59701721133853E-17,1.,4.16333634234433E-17));
#16075=DIRECTION('ref_axis',(-4.30625898502832E-33,-4.16333634234433E-17,
1.));
#16076=DIRECTION('',(4.59701721133853E-17,1.,4.16333634234433E-17));
#16077=DIRECTION('center_axis',(9.57910591987181E-15,-0.707106781186552,
0.707106781186543));
#16078=DIRECTION('ref_axis',(3.75170549529962E-13,-0.707106781186543,-0.707106781186552));
#16079=DIRECTION('center_axis',(-1.16018306073329E-14,5.63785129692462E-17,
1.));
#16080=DIRECTION('ref_axis',(1.,5.8113236445223E-17,1.16018306073329E-14));
#16081=DIRECTION('',(4.59701721133853E-17,1.,4.16333634234433E-17));
#16082=DIRECTION('',(1.,1.17015772072015E-14,1.16018306073329E-14));
#16083=DIRECTION('center_axis',(4.59701721133853E-17,1.,4.16333634234433E-17));
#16084=DIRECTION('ref_axis',(-4.30625898502839E-33,-4.16333634234433E-17,
1.));
#16085=DIRECTION('',(4.59701721133853E-17,1.,4.16333634234433E-17));
#16086=DIRECTION('center_axis',(2.87774982255266E-14,0.70710678118654,-0.707106781186555));
#16087=DIRECTION('ref_axis',(-1.67738755276477E-12,0.707106781186555,0.70710678118654));
#16088=DIRECTION('center_axis',(-1.,-4.9439619065339E-17,-7.71605002114484E-15));
#16089=DIRECTION('ref_axis',(-7.71605002114484E-15,6.33174068731535E-17,
1.));
#16090=DIRECTION('',(4.59701721133853E-17,1.,4.16333634234433E-17));
#16091=DIRECTION('',(-5.71764857681955E-15,0.707106781186548,0.707106781186547));
#16092=DIRECTION('center_axis',(4.59701721133853E-17,1.,4.16333634234433E-17));
#16093=DIRECTION('ref_axis',(-4.3062589850284E-33,-4.16333634234433E-17,
1.));
#16094=DIRECTION('',(4.59701721133853E-17,1.,4.16333634234433E-17));
#16095=DIRECTION('center_axis',(-6.92543468531269E-14,-0.707106781186525,
0.70710678118657));
#16096=DIRECTION('ref_axis',(-5.72091053931135E-13,-0.70710678118657,-0.707106781186525));
#16097=DIRECTION('center_axis',(5.55111512312578E-17,5.20417042793042E-17,
1.));
#16098=DIRECTION('ref_axis',(1.,4.77048955893622E-17,-5.55111512312578E-17));
#16099=DIRECTION('',(4.59701721133853E-17,1.,4.16333634234433E-17));
#16100=DIRECTION('',(1.,4.77048955893622E-17,-5.55111512312578E-17));
#16101=DIRECTION('center_axis',(1.,5.03069808033274E-17,1.09356967925578E-14));
#16102=DIRECTION('ref_axis',(1.09356967925578E-14,-5.89805981832114E-17,
-1.));
#16103=DIRECTION('',(7.82707232360735E-15,-0.707106781186548,-0.707106781186547));
#16104=DIRECTION('center_axis',(-1.66533453693774E-16,-0.707106781186547,
0.707106781186548));
#16105=DIRECTION('ref_axis',(2.77555756156289E-16,-0.707106781186548,-0.707106781186547));
#16106=DIRECTION('center_axis',(1.,1.0769163338864E-14,-1.46936793852784E-39));
#16107=DIRECTION('ref_axis',(-1.0769163338864E-14,1.,6.61744490042422E-24));
#16108=DIRECTION('',(-7.43849426498854E-15,0.707106781186548,-0.707106781186547));
#16109=DIRECTION('',(0.,-1.32348898008484E-23,-1.));
#16110=DIRECTION('',(7.4940054162198E-15,-0.707106781186548,-0.707106781186547));
#16111=DIRECTION('',(0.,-1.32348898008484E-23,-1.));
#16112=DIRECTION('center_axis',(0.,1.,-1.32348898008484E-23));
#16113=DIRECTION('ref_axis',(0.,1.32348898008484E-23,1.));
#16114=DIRECTION('',(-1.,-1.66533453693773E-16,1.32348898008484E-23));
#16115=DIRECTION('',(0.,-1.32348898008484E-23,-1.));
#16116=DIRECTION('',(1.,1.66533453693773E-16,-1.32348898008484E-23));
#16117=DIRECTION('center_axis',(0.,-1.32348898008484E-23,-1.));
#16118=DIRECTION('ref_axis',(-1.,0.,0.));
#16119=DIRECTION('center_axis',(7.7668426377335E-15,-0.707106781186543,
-0.707106781186552));
#16120=DIRECTION('ref_axis',(-1.50420492628612E-12,0.707106781186552,-0.707106781186543));
#16121=DIRECTION('',(0.,-1.32348898008484E-23,-1.));
#16122=DIRECTION('center_axis',(-8.47880321285962E-15,-0.707106781186537,
0.707106781186558));
#16123=DIRECTION('ref_axis',(-1.33652306564903E-12,-0.707106781186558,-0.707106781186537));
#16124=DIRECTION('center_axis',(-1.,-7.66053886991358E-15,6.61744490042422E-24));
#16125=DIRECTION('ref_axis',(7.66053886991358E-15,-1.,-3.97046694025453E-23));
#16126=DIRECTION('',(5.21804821573823E-15,-0.707106781186548,0.707106781186547));
#16127=DIRECTION('',(0.,-1.32348898008484E-23,-1.));
#16128=DIRECTION('',(-5.27355936696949E-15,0.707106781186548,0.707106781186547));
#16129=DIRECTION('center_axis',(0.,-1.32348898008484E-23,-1.));
#16130=DIRECTION('ref_axis',(-1.,0.,0.));
#16131=DIRECTION('center_axis',(2.62788531700192E-14,0.707106781186538,
0.707106781186557));
#16132=DIRECTION('ref_axis',(-1.00193785715871E-13,-0.707106781186557,0.707106781186538));
#16133=DIRECTION('',(0.,-1.32348898008484E-23,-1.));
#16134=DIRECTION('center_axis',(1.15454633599422E-14,0.707106781186547,
-0.707106781186548));
#16135=DIRECTION('ref_axis',(-1.20981655275665E-12,0.707106781186548,0.707106781186547));
#16136=DIRECTION('center_axis',(-1.17128529097954E-14,1.,2.64697796016969E-23));
#16137=DIRECTION('ref_axis',(-1.,-1.17128529097954E-14,0.));
#16138=DIRECTION('',(-1.,-1.17128529097954E-14,1.16517419311056E-14));
#16139=DIRECTION('',(0.,-1.32348898008484E-23,-1.));
#16140=DIRECTION('',(1.,1.17128529097954E-14,1.16517419311056E-14));
#16141=DIRECTION('center_axis',(0.,-1.32348898008484E-23,-1.));
#16142=DIRECTION('ref_axis',(-1.,0.,0.));
#16143=DIRECTION('center_axis',(1.37214219933299E-14,-0.70710678118655,
-0.707106781186545));
#16144=DIRECTION('ref_axis',(-1.13009119520484E-12,0.707106781186545,-0.70710678118655));
#16145=DIRECTION('',(0.,-1.32348898008484E-23,-1.));
#16146=DIRECTION('center_axis',(2.9902344155278E-14,-0.707106781186557,
0.707106781186538));
#16147=DIRECTION('ref_axis',(-1.59121631194934E-12,-0.707106781186538,-0.707106781186557));
#16148=DIRECTION('center_axis',(-1.,-1.66533453693773E-16,2.20405190779179E-39));
#16149=DIRECTION('ref_axis',(0.,1.32348898008484E-23,1.));
#16150=DIRECTION('',(-2.22044604925031E-16,-0.707106781186548,0.707106781186547));
#16151=DIRECTION('',(0.,-1.32348898008484E-23,-1.));
#16152=DIRECTION('',(1.66533453693773E-16,0.707106781186548,0.707106781186547));
#16153=DIRECTION('center_axis',(1.04360964314765E-14,-1.,0.));
#16154=DIRECTION('ref_axis',(1.,1.04360964314765E-14,0.));
#16155=DIRECTION('',(1.,1.04360964314765E-14,-1.03810223757158E-14));
#16156=DIRECTION('',(-1.,-1.04360964314765E-14,-1.03810223757158E-14));
#16157=DIRECTION('center_axis',(-1.11022302462516E-16,-0.707106781186547,
0.707106781186548));
#16158=DIRECTION('ref_axis',(-1.66533453693773E-16,-0.707106781186548,-0.707106781186547));
#16159=DIRECTION('center_axis',(-1.66533453693773E-16,-0.707106781186547,
-0.707106781186548));
#16160=DIRECTION('ref_axis',(2.22044604925031E-16,0.707106781186548,-0.707106781186547));
#16161=DIRECTION('center_axis',(-7.8062556418956E-18,-1.,-9.19403442267707E-17));
#16162=DIRECTION('ref_axis',(4.44089209850062E-16,9.19403442267707E-17,
-1.));
#16163=DIRECTION('',(1.06026298851702E-14,-1.45716771982052E-16,1.));
#16164=DIRECTION('',(-1.,-1.21430643318376E-17,1.08246744900953E-14));
#16165=DIRECTION('',(4.44089209850062E-16,1.50920942409982E-16,-1.));
#16166=DIRECTION('center_axis',(7.80625564189562E-18,1.,4.07660016854549E-17));
#16167=DIRECTION('ref_axis',(-3.99480000183453E-34,4.07660016854549E-17,
-1.));
#16168=DIRECTION('',(1.,1.47451495458029E-17,-1.19904086659517E-14));
#16169=DIRECTION('center_axis',(-7.80625564189562E-18,-1.,-4.07660016854549E-17));
#16170=DIRECTION('ref_axis',(-3.99480000183441E-34,4.07660016854549E-17,
-1.));
#16171=DIRECTION('',(-7.32747196252603E-15,1.50920942409982E-16,-1.));
#16172=DIRECTION('center_axis',(7.80625564189562E-18,1.,4.07660016854549E-17));
#16173=DIRECTION('ref_axis',(3.99480000183447E-34,-4.07660016854549E-17,
1.));
#16174=DIRECTION('',(1.,1.73472347597681E-17,-3.33066907387547E-16));
#16175=DIRECTION('center_axis',(1.08246744900953E-14,-3.20923843055709E-17,
1.));
#16176=DIRECTION('ref_axis',(1.,1.21430643318377E-17,-1.08246744900953E-14));
#16177=DIRECTION('',(-1.21430643318376E-17,-1.,2.60208521396521E-17));
#16178=DIRECTION('',(1.,1.03866568124111E-14,-1.0769163338864E-14));
#16179=DIRECTION('',(-1.21430643318376E-17,-1.,2.60208521396521E-17));
#16180=DIRECTION('center_axis',(-1.,-1.7347234759768E-17,-4.44089209850062E-16));
#16181=DIRECTION('ref_axis',(-4.44089209850062E-16,-2.94902990916057E-17,
1.));
#16182=DIRECTION('',(-2.77555756156289E-16,-0.707106781186548,0.707106781186547));
#16183=DIRECTION('',(-1.21430643318376E-17,-1.,2.60208521396521E-17));
#16184=DIRECTION('center_axis',(-1.21430643318376E-17,-1.,2.60208521396521E-17));
#16185=DIRECTION('ref_axis',(-3.1597288150103E-34,-2.60208521396521E-17,
-1.));
#16186=DIRECTION('center_axis',(-1.13913692020097E-14,-0.707106781186534,
-0.707106781186561));
#16187=DIRECTION('ref_axis',(1.83534137375699E-13,0.707106781186561,-0.707106781186534));
#16188=DIRECTION('',(-1.21430643318376E-17,-1.,2.60208521396521E-17));
#16189=DIRECTION('center_axis',(-1.19904086659517E-14,2.08166817117216E-17,
-1.));
#16190=DIRECTION('ref_axis',(-1.,-1.82145964977565E-17,1.19904086659517E-14));
#16191=DIRECTION('',(-1.,-1.1669484822896E-14,1.21569421196455E-14));
#16192=DIRECTION('',(-1.21430643318376E-17,-1.,2.60208521396521E-17));
#16193=DIRECTION('center_axis',(-1.21430643318376E-17,-1.,2.60208521396521E-17));
#16194=DIRECTION('ref_axis',(-3.1597288150103E-34,-2.60208521396521E-17,
-1.));
#16195=DIRECTION('center_axis',(1.37856278924687E-14,0.707106781186535,
0.70710678118656));
#16196=DIRECTION('ref_axis',(-8.00926025379328E-13,-0.70710678118656,0.707106781186535));
#16197=DIRECTION('',(-1.21430643318376E-17,-1.,2.60208521396521E-17));
#16198=DIRECTION('center_axis',(-1.,-1.3010426069826E-17,7.32747196252603E-15));
#16199=DIRECTION('ref_axis',(7.32747196252603E-15,-2.60208521396521E-17,
1.));
#16200=DIRECTION('',(5.10702591327571E-15,-0.707106781186548,0.707106781186547));
#16201=DIRECTION('',(-1.21430643318376E-17,-1.,2.60208521396521E-17));
#16202=DIRECTION('center_axis',(-1.21430643318376E-17,-1.,2.60208521396521E-17));
#16203=DIRECTION('ref_axis',(-3.1597288150103E-34,-2.60208521396521E-17,
-1.));
#16204=DIRECTION('center_axis',(-3.88342131886675E-15,-0.70710678118655,
-0.707106781186545));
#16205=DIRECTION('ref_axis',(-1.83322773685989E-12,0.707106781186545,-0.70710678118655));
#16206=DIRECTION('',(-1.21430643318376E-17,-1.,2.60208521396521E-17));
#16207=DIRECTION('center_axis',(-3.33066907387547E-16,2.94902990916057E-17,
-1.));
#16208=DIRECTION('ref_axis',(-1.,-1.73472347597681E-17,3.33066907387547E-16));
#16209=DIRECTION('',(-1.,-1.73472347597681E-17,3.33066907387547E-16));
#16210=DIRECTION('',(-1.21430643318376E-17,-1.,2.60208521396521E-17));
#16211=DIRECTION('center_axis',(1.,2.42861286636753E-17,-1.06026298851702E-14));
#16212=DIRECTION('ref_axis',(-1.06026298851702E-14,2.42861286636753E-17,
-1.));
#16213=DIRECTION('',(-7.27196081129477E-15,0.707106781186548,-0.707106781186547));
#16214=DIRECTION('center_axis',(3.33066907387547E-16,-0.707106781186547,
-0.707106781186548));
#16215=DIRECTION('ref_axis',(2.77555756156289E-16,0.707106781186548,-0.707106781186547));
#16216=DIRECTION('center_axis',(1.30104260698256E-17,-1.,-2.51534904016636E-17));
#16217=DIRECTION('ref_axis',(-6.93889390390723E-15,-2.51534904016637E-17,
1.));
#16218=DIRECTION('',(-3.88578058618805E-15,-2.60208521396521E-17,-1.));
#16219=DIRECTION('',(1.,-1.3010426069826E-17,-3.38618022510673E-15));
#16220=DIRECTION('',(-6.93889390390723E-15,3.72965547335013E-17,1.));
#16221=DIRECTION('center_axis',(-1.3010426069826E-17,1.,8.8470897274817E-17));
#16222=DIRECTION('ref_axis',(8.23786441056261E-34,-8.8470897274817E-17,
1.));
#16223=DIRECTION('',(-1.,1.64798730217797E-17,4.77395900588817E-15));
#16224=DIRECTION('center_axis',(1.3010426069826E-17,-1.,-8.8470897274817E-17));
#16225=DIRECTION('ref_axis',(8.23786441056244E-34,-8.8470897274817E-17,
1.));
#16226=DIRECTION('',(7.21644966006352E-16,3.55618312575245E-17,1.));
#16227=DIRECTION('center_axis',(-1.3010426069826E-17,1.,8.8470897274817E-17));
#16228=DIRECTION('ref_axis',(-8.23786441056256E-34,8.8470897274817E-17,
-1.));
#16229=DIRECTION('',(-1.,1.73472347597681E-17,-7.04991620636974E-15));
#16230=DIRECTION('center_axis',(-3.38618022510673E-15,-3.64291929955129E-17,
-1.));
#16231=DIRECTION('ref_axis',(-1.,1.3010426069826E-17,3.38618022510673E-15));
#16232=DIRECTION('',(1.21430643318376E-17,-1.,-2.77555756156289E-17));
#16233=DIRECTION('',(-1.,4.73926453636863E-15,3.38618022510672E-15));
#16234=DIRECTION('',(1.21430643318376E-17,-1.,-2.77555756156289E-17));
#16235=DIRECTION('center_axis',(1.,-1.73472347597681E-17,6.93889390390723E-15));
#16236=DIRECTION('ref_axis',(6.93889390390723E-15,-3.72965547335013E-17,
-1.));
#16237=DIRECTION('',(4.88498130835068E-15,-0.707106781186548,-0.707106781186548));
#16238=DIRECTION('',(1.21430643318376E-17,-1.,-2.77555756156289E-17));
#16239=DIRECTION('center_axis',(1.21430643318376E-17,-1.,-2.77555756156289E-17));
#16240=DIRECTION('ref_axis',(-3.37037740267765E-34,2.77555756156289E-17,
-1.));
#16241=DIRECTION('center_axis',(-3.52096866244013E-14,-0.707106781186563,
0.707106781186532));
#16242=DIRECTION('ref_axis',(4.00992146975888E-12,-0.707106781186532,-0.707106781186563));
#16243=DIRECTION('',(1.21430643318376E-17,-1.,-2.77555756156289E-17));
#16244=DIRECTION('center_axis',(4.49640324973188E-15,3.46944695195361E-17,
1.));
#16245=DIRECTION('ref_axis',(1.,-1.21430643318376E-17,-4.49640324973188E-15));
#16246=DIRECTION('',(1.,-6.00648003556969E-15,-4.94049245958194E-15));
#16247=DIRECTION('',(1.21430643318376E-17,-1.,-2.77555756156289E-17));
#16248=DIRECTION('center_axis',(1.21430643318376E-17,-1.,-2.77555756156289E-17));
#16249=DIRECTION('ref_axis',(-3.37037740267765E-34,2.77555756156289E-17,
-1.));
#16250=DIRECTION('center_axis',(7.75441568951419E-16,0.707106781186544,
-0.707106781186551));
#16251=DIRECTION('ref_axis',(-7.1228105608578E-13,0.707106781186551,0.707106781186544));
#16252=DIRECTION('',(1.21430643318376E-17,-1.,-2.77555756156289E-17));
#16253=DIRECTION('center_axis',(1.,-1.56125112837912E-17,-7.21644966006352E-16));
#16254=DIRECTION('ref_axis',(-7.21644966006352E-16,-3.55618312575245E-17,
-1.));
#16255=DIRECTION('',(-5.55111512312578E-16,-0.707106781186548,-0.707106781186547));
#16256=DIRECTION('',(1.21430643318376E-17,-1.,-2.77555756156289E-17));
#16257=DIRECTION('center_axis',(1.21430643318376E-17,-1.,-2.77555756156289E-17));
#16258=DIRECTION('ref_axis',(-3.37037740267765E-34,2.77555756156289E-17,
-1.));
#16259=DIRECTION('center_axis',(1.2168053465783E-14,-0.707106781186539,
0.707106781186556));
#16260=DIRECTION('ref_axis',(4.94238761493454E-13,-0.707106781186556,-0.707106781186539));
#16261=DIRECTION('',(1.21430643318376E-17,-1.,-2.77555756156289E-17));
#16262=DIRECTION('center_axis',(-7.04991620636974E-15,3.72965547335013E-17,
1.));
#16263=DIRECTION('ref_axis',(1.,-1.73472347597681E-17,7.04991620636974E-15));
#16264=DIRECTION('',(1.,5.62137142390284E-15,7.4940054162198E-15));
#16265=DIRECTION('',(1.21430643318376E-17,-1.,-2.77555756156289E-17));
#16266=DIRECTION('center_axis',(-1.,1.99493199737333E-17,3.88578058618805E-15));
#16267=DIRECTION('ref_axis',(3.88578058618805E-15,2.60208521396521E-17,
1.));
#16268=DIRECTION('',(2.77555756156289E-15,0.707106781186548,0.707106781186548));
#16269=DIRECTION('center_axis',(-8.32667268468867E-16,-0.707106781186548,
0.707106781186548));
#16270=DIRECTION('ref_axis',(-2.22044604925031E-16,-0.707106781186548,-0.707106781186548));
#16271=DIRECTION('center_axis',(-1.,5.44009282066327E-15,-1.33226766263741E-15));
#16272=DIRECTION('ref_axis',(-5.44009282066327E-15,-1.,4.63221143029696E-23));
#16273=DIRECTION('',(-4.71844785465691E-15,-0.707106781186548,0.707106781186548));
#16274=DIRECTION('',(-1.33226760969785E-15,-1.11022342167185E-16,1.));
#16275=DIRECTION('',(2.94209101525666E-15,0.707106781186547,0.707106781186548));
#16276=DIRECTION('',(-1.33226760969785E-15,-1.11022342167185E-16,1.));
#16277=DIRECTION('center_axis',(-5.6621374255883E-15,1.,1.11022223053177E-16));
#16278=DIRECTION('ref_axis',(-1.,-5.6621374255883E-15,-1.32348898008484E-23));
#16279=DIRECTION('',(-1.,-5.6621374255883E-15,5.15950545417941E-15));
#16280=DIRECTION('',(1.,5.6621374255883E-15,6.98296269881226E-15));
#16281=DIRECTION('',(-1.33226760969785E-15,-1.11022342167185E-16,1.));
#16282=DIRECTION('center_axis',(-1.33226760969785E-15,-1.11022342167185E-16,
1.));
#16283=DIRECTION('ref_axis',(1.,-1.47911470422133E-31,1.33226760969785E-15));
#16284=DIRECTION('center_axis',(2.59541991477666E-14,-0.707106781186537,
-0.707106781186559));
#16285=DIRECTION('ref_axis',(-1.63630723245591E-12,0.707106781186559,-0.707106781186536));
#16286=DIRECTION('center_axis',(1.21680534657822E-14,-0.70710678118654,
0.707106781186555));
#16287=DIRECTION('ref_axis',(-2.30210285556933E-12,-0.707106781186556,-0.707106781186539));
#16288=DIRECTION('',(-1.33226760969785E-15,-1.11022342167185E-16,1.));
#16289=DIRECTION('center_axis',(1.,-2.22044604925031E-15,1.33226765601997E-15));
#16290=DIRECTION('ref_axis',(2.22044604925031E-15,1.,-1.98523347012727E-23));
#16291=DIRECTION('',(2.4980018054066E-15,0.707106781186548,-0.707106781186547));
#16292=DIRECTION('',(-6.66133814775094E-16,-0.707106781186547,-0.707106781186548));
#16293=DIRECTION('',(-1.33226760969785E-15,-1.11022342167185E-16,1.));
#16294=DIRECTION('center_axis',(-1.33226760969785E-15,-1.11022342167185E-16,
1.));
#16295=DIRECTION('ref_axis',(1.,-1.47911470422133E-31,1.33226760969785E-15));
#16296=DIRECTION('center_axis',(-1.72320348655873E-14,0.70710678118654,
0.707106781186555));
#16297=DIRECTION('ref_axis',(1.75729287719648E-12,-0.707106781186555,0.70710678118654));
#16298=DIRECTION('center_axis',(-9.0468183044332E-15,0.707106781186546,
-0.707106781186549));
#16299=DIRECTION('ref_axis',(-6.90431943935876E-13,0.707106781186549,0.707106781186546));
#16300=DIRECTION('',(-1.33226760969785E-15,-1.11022342167185E-16,1.));
#16301=DIRECTION('center_axis',(5.93969318174459E-15,1.,1.11022242905512E-16));
#16302=DIRECTION('ref_axis',(-1.,5.93969318174459E-15,-1.32348898008484E-23));
#16303=DIRECTION('',(-1.,5.93969318174459E-15,-6.4922364769262E-15));
#16304=DIRECTION('',(1.,-5.93969318174459E-15,-4.66877923229335E-15));
#16305=DIRECTION('',(-1.33226760969785E-15,-1.11022342167185E-16,1.));
#16306=DIRECTION('center_axis',(-1.33226760969785E-15,-1.11022342167185E-16,
1.));
#16307=DIRECTION('ref_axis',(1.,-1.47911470422133E-31,1.33226760969785E-15));
#16308=DIRECTION('center_axis',(-1.35919746160361E-14,-0.70710678118655,
-0.707106781186545));
#16309=DIRECTION('ref_axis',(-1.90544366423202E-12,0.707106781186545,-0.70710678118655));
#16310=DIRECTION('center_axis',(-1.91582118397469E-14,-0.707106781186557,
0.707106781186538));
#16311=DIRECTION('ref_axis',(6.31977432729113E-13,-0.707106781186538,-0.707106781186557));
#16312=DIRECTION('',(-1.33226760969785E-15,-1.11022342167185E-16,1.));
#16313=DIRECTION('center_axis',(1.,5.60662627435704E-15,1.33226764278508E-15));
#16314=DIRECTION('ref_axis',(-5.60662627435704E-15,1.,-5.29395592033938E-23));
#16315=DIRECTION('',(-3.10862446895044E-15,0.707106781186548,-0.707106781186548));
#16316=DIRECTION('',(4.88498130835069E-15,-0.707106781186547,-0.707106781186548));
#16317=DIRECTION('',(-1.33226760969785E-15,-1.11022342167185E-16,1.));
#16318=DIRECTION('center_axis',(-4.6074255521944E-15,-1.,-1.11022249522956E-16));
#16319=DIRECTION('ref_axis',(1.,-4.6074255521944E-15,2.64697796016969E-23));
#16320=DIRECTION('',(1.,-4.6074255521944E-15,5.22151693477125E-15));
#16321=DIRECTION('',(-1.,4.6074255521944E-15,3.39805966366862E-15));
#16322=DIRECTION('center_axis',(-9.9920072216264E-16,-0.707106781186548,
0.707106781186547));
#16323=DIRECTION('ref_axis',(-1.66533453693773E-16,-0.707106781186547,-0.707106781186548));
#16324=DIRECTION('center_axis',(3.88578058618804E-16,-0.707106781186547,
-0.707106781186548));
#16325=DIRECTION('ref_axis',(1.11022302462516E-16,0.707106781186548,-0.707106781186547));
#16326=DIRECTION('center_axis',(8.35269353682832E-16,1.,1.84748050191525E-16));
#16327=DIRECTION('ref_axis',(-5.27355936696949E-15,1.8474805019153E-16,
-1.));
#16328=DIRECTION('',(-5.6621374255883E-15,-1.25767452008318E-16,1.));
#16329=DIRECTION('',(-1.,8.52616588442601E-16,5.10702591327572E-15));
#16330=DIRECTION('center_axis',(-8.35269353682832E-16,-1.,-1.82145964977565E-16));
#16331=DIRECTION('ref_axis',(2.17344203489769E-33,-1.82145964977565E-16,
1.));
#16332=DIRECTION('',(2.55351295663786E-15,1.22298005056365E-16,-1.));
#16333=DIRECTION('center_axis',(8.35269353682832E-16,1.,1.82145964977565E-16));
#16334=DIRECTION('ref_axis',(-2.17344203489616E-33,1.82145964977565E-16,
-1.));
#16335=DIRECTION('',(-1.,8.44810332800705E-16,-6.60582699651968E-15));
#16336=DIRECTION('center_axis',(-8.35269353682832E-16,-1.,-1.82145964977565E-16));
#16337=DIRECTION('ref_axis',(-2.17344203489581E-33,1.82145964977565E-16,
-1.));
#16338=DIRECTION('',(-5.27355936696949E-15,1.25767452008318E-16,-1.));
#16339=DIRECTION('',(1.,-8.4741241801467E-16,5.21804821573823E-15));
#16340=DIRECTION('center_axis',(-5.16253706450698E-15,-1.05818132034585E-16,
1.));
#16341=DIRECTION('ref_axis',(1.,-8.67361737988404E-18,5.16253706450698E-15));
#16342=DIRECTION('',(8.32667268468867E-16,1.,1.02348685082632E-16));
#16343=DIRECTION('',(1.,-4.73406036594071E-15,5.21804821573824E-15));
#16344=DIRECTION('',(8.32667268468867E-16,1.,1.02348685082632E-16));
#16345=DIRECTION('center_axis',(1.,-8.52616588442601E-16,-5.27355936696949E-15));
#16346=DIRECTION('ref_axis',(-5.27355936696949E-15,4.33680868994202E-18,
-1.));
#16347=DIRECTION('',(8.32667268468867E-16,1.,1.02348685082632E-16));
#16348=DIRECTION('',(-3.10862446895044E-15,0.707106781186548,-0.707106781186547));
#16349=DIRECTION('center_axis',(8.32667268468867E-16,1.,1.02348685082632E-16));
#16350=DIRECTION('ref_axis',(-1.,8.32667268468867E-16,-1.86424000085681E-33));
#16351=DIRECTION('',(8.32667268468867E-16,1.,1.02348685082632E-16));
#16352=DIRECTION('center_axis',(8.47880321285959E-15,-0.707106781186537,
-0.707106781186558));
#16353=DIRECTION('ref_axis',(2.64873930696695E-12,0.707106781186558,-0.707106781186537));
#16354=DIRECTION('center_axis',(6.60582699651968E-15,1.00613961606655E-16,
-1.));
#16355=DIRECTION('ref_axis',(-1.,1.12757025938492E-17,-6.60582699651968E-15));
#16356=DIRECTION('',(8.32667268468867E-16,1.,1.02348685082632E-16));
#16357=DIRECTION('',(-1.,6.00387795035573E-15,-6.60582699651968E-15));
#16358=DIRECTION('center_axis',(8.32667268468867E-16,1.,1.02348685082632E-16));
#16359=DIRECTION('ref_axis',(-1.,8.32667268468867E-16,-1.86424000085607E-33));
#16360=DIRECTION('',(8.32667268468867E-16,1.,1.02348685082632E-16));
#16361=DIRECTION('center_axis',(-8.27137673548193E-15,0.707106781186542,
0.707106781186553));
#16362=DIRECTION('ref_axis',(-2.01011831778871E-13,-0.707106781186553,0.707106781186542));
#16363=DIRECTION('center_axis',(1.,-8.49147141490647E-16,2.55351295663786E-15));
#16364=DIRECTION('ref_axis',(2.55351295663786E-15,-2.60208521396521E-18,
-1.));
#16365=DIRECTION('',(8.32667268468867E-16,1.,1.02348685082632E-16));
#16366=DIRECTION('',(2.55351295663786E-15,0.707106781186548,-0.707106781186547));
#16367=DIRECTION('center_axis',(8.32667268468867E-16,1.,1.02348685082632E-16));
#16368=DIRECTION('ref_axis',(-1.,8.32667268468867E-16,-1.86424000085454E-33));
#16369=DIRECTION('',(8.32667268468867E-16,1.,1.02348685082632E-16));
#16370=DIRECTION('center_axis',(5.56623722370933E-15,-0.707106781186541,
-0.707106781186554));
#16371=DIRECTION('ref_axis',(-4.75568302221126E-13,0.707106781186554,-0.707106781186541));
#16372=DIRECTION('center_axis',(-5.10702591327572E-15,1.0842021724855E-16,
-1.));
#16373=DIRECTION('ref_axis',(-1.,1.12757025938492E-17,5.10702591327572E-15));
#16374=DIRECTION('',(8.32667268468867E-16,1.,1.02348685082632E-16));
#16375=DIRECTION('',(-1.,-5.6395860204006E-15,5.27355936696949E-15));
#16376=DIRECTION('center_axis',(-1.,8.45677694538693E-16,-5.6621374255883E-15));
#16377=DIRECTION('ref_axis',(-5.6621374255883E-15,-4.33680868994202E-18,
1.));
#16378=DIRECTION('',(-4.71844785465692E-15,-0.707106781186548,0.707106781186547));
#16379=DIRECTION('center_axis',(3.88578058618805E-16,-0.707106781186547,
-0.707106781186548));
#16380=DIRECTION('ref_axis',(1.11022302462516E-16,0.707106781186548,-0.707106781186547));
#16381=DIRECTION('center_axis',(-1.0345260002189E-14,1.,0.));
#16382=DIRECTION('ref_axis',(-1.,-1.0345260002189E-14,0.));
#16383=DIRECTION('center_axis',(-1.0345260002189E-14,1.,0.));
#16384=DIRECTION('ref_axis',(-1.,-1.0345260002189E-14,0.));
#16385=DIRECTION('',(-1.0345260002189E-14,1.,0.));
#16386=DIRECTION('center_axis',(-1.0345260002189E-14,1.,0.));
#16387=DIRECTION('ref_axis',(-1.,-1.0345260002189E-14,0.));
#16388=DIRECTION('',(-1.0345260002189E-14,1.,0.));
#16389=DIRECTION('center_axis',(-1.0345260002189E-14,1.,0.));
#16390=DIRECTION('ref_axis',(-1.,-1.0345260002189E-14,0.));
#16391=DIRECTION('center_axis',(-1.0345260002189E-14,1.,0.));
#16392=DIRECTION('ref_axis',(-1.,-1.0345260002189E-14,0.));
#16393=DIRECTION('',(-1.0345260002189E-14,1.,0.));
#16394=DIRECTION('center_axis',(-1.0345260002189E-14,1.,0.));
#16395=DIRECTION('ref_axis',(-1.,-1.0345260002189E-14,0.));
#16396=DIRECTION('',(-1.0345260002189E-14,1.,0.));
#16397=DIRECTION('center_axis',(-1.0345260002189E-14,1.,0.));
#16398=DIRECTION('ref_axis',(-1.,-1.0345260002189E-14,0.));
#16399=DIRECTION('center_axis',(-1.0345260002189E-14,1.,0.));
#16400=DIRECTION('ref_axis',(-1.,-1.0345260002189E-14,0.));
#16401=DIRECTION('',(-1.0345260002189E-14,1.,0.));
#16402=DIRECTION('center_axis',(-1.0345260002189E-14,1.,0.));
#16403=DIRECTION('ref_axis',(-1.,-1.0345260002189E-14,0.));
#16404=DIRECTION('',(-1.0345260002189E-14,1.,0.));
#16405=DIRECTION('center_axis',(-1.0345260002189E-14,1.,0.));
#16406=DIRECTION('ref_axis',(-1.,-1.0345260002189E-14,0.));
#16407=DIRECTION('center_axis',(-1.0345260002189E-14,1.,0.));
#16408=DIRECTION('ref_axis',(-1.,-1.0345260002189E-14,0.));
#16409=DIRECTION('',(-1.0345260002189E-14,1.,0.));
#16410=DIRECTION('center_axis',(-1.0345260002189E-14,1.,0.));
#16411=DIRECTION('ref_axis',(-1.,-1.0345260002189E-14,0.));
#16412=DIRECTION('',(-1.0345260002189E-14,1.,0.));
#16413=DIRECTION('center_axis',(1.,1.03805852802452E-14,0.));
#16414=DIRECTION('ref_axis',(-1.03805852802452E-14,1.,0.));
#16415=DIRECTION('',(0.,0.,1.));
#16416=DIRECTION('',(-1.03805852802452E-14,1.,1.32348898008484E-23));
#16417=DIRECTION('',(0.,0.,1.));
#16418=DIRECTION('',(1.03805852802452E-14,-1.,-1.32348898008484E-23));
#16419=DIRECTION('center_axis',(-1.36918376090096E-37,1.32348898008484E-23,
-1.));
#16420=DIRECTION('ref_axis',(0.,1.,1.32348898008484E-23));
#16421=DIRECTION('',(1.,1.0345260002189E-14,0.));
#16422=DIRECTION('',(1.03805852802452E-14,-1.,-1.32348898008484E-23));
#16423=DIRECTION('',(1.,1.0345260002189E-14,0.));
#16424=DIRECTION('',(-1.03805852802452E-14,1.,1.32348898008484E-23));
#16425=DIRECTION('center_axis',(-1.,-1.03805852802452E-14,0.));
#16426=DIRECTION('ref_axis',(1.03805852802452E-14,-1.,0.));
#16427=DIRECTION('',(0.,0.,-1.));
#16428=DIRECTION('',(-1.03805852802452E-14,1.,1.32348898008484E-23));
#16429=DIRECTION('',(0.,0.,-1.));
#16430=DIRECTION('',(1.03805852802452E-14,-1.,-1.32348898008484E-23));
#16431=DIRECTION('center_axis',(1.36918376090096E-37,-1.32348898008484E-23,
1.));
#16432=DIRECTION('ref_axis',(0.,-1.,-1.32348898008484E-23));
#16433=DIRECTION('',(-1.,-1.0345260002189E-14,0.));
#16434=DIRECTION('',(-1.03805852802452E-14,1.,1.32348898008484E-23));
#16435=DIRECTION('',(-1.,-1.0345260002189E-14,0.));
#16436=DIRECTION('',(1.03805852802452E-14,-1.,-1.32348898008484E-23));
#16437=DIRECTION('center_axis',(1.0345260002189E-14,-1.,0.));
#16438=DIRECTION('ref_axis',(1.,1.0345260002189E-14,0.));
#16439=DIRECTION('',(0.707106781186544,7.31520350068574E-15,0.70710678118655));
#16440=DIRECTION('',(0.707106781186551,7.31520350068581E-15,-0.707106781186544));
#16441=DIRECTION('',(-0.707106781186549,-7.31520350068578E-15,-0.707106781186547));
#16442=DIRECTION('',(-0.707106781186549,-7.31520350068579E-15,0.707106781186546));
#16443=DIRECTION('',(1.,1.11022302462513E-14,0.));
#16444=DIRECTION('',(-1.,-1.11022302462516E-14,0.));
#16445=DIRECTION('center_axis',(-1.0345260002189E-14,1.,0.));
#16446=DIRECTION('ref_axis',(-1.,-1.0345260002189E-14,0.));
#16447=DIRECTION('',(1.,1.11022302462513E-14,0.));
#16448=DIRECTION('',(-1.,-1.11022302462516E-14,0.));
#16449=DIRECTION('center_axis',(-1.0345260002189E-14,1.,0.));
#16450=DIRECTION('ref_axis',(-1.,-1.0345260002189E-14,0.));
#16451=DIRECTION('',(1.,1.11022302462513E-14,0.));
#16452=DIRECTION('',(-1.,-1.11022302462516E-14,0.));
#16453=DIRECTION('center_axis',(-1.0345260002189E-14,1.,0.));
#16454=DIRECTION('ref_axis',(-1.,-1.0345260002189E-14,0.));
#16455=DIRECTION('',(1.,1.11022302462513E-14,0.));
#16456=DIRECTION('',(-1.,-1.11022302462516E-14,0.));
#16457=DIRECTION('center_axis',(-1.0345260002189E-14,1.,0.));
#16458=DIRECTION('ref_axis',(-1.,-1.0345260002189E-14,0.));
#16459=DIRECTION('center_axis',(1.0345260002189E-14,-1.,0.));
#16460=DIRECTION('ref_axis',(1.,1.0345260002189E-14,0.));
#16461=DIRECTION('',(-0.707106781186544,-7.31520350068574E-15,-0.70710678118655));
#16462=DIRECTION('',(0.707106781186549,7.31520350068579E-15,-0.707106781186546));
#16463=DIRECTION('',(0.707106781186549,7.31520350068578E-15,0.707106781186546));
#16464=DIRECTION('',(-0.707106781186551,-7.31520350068581E-15,0.707106781186544));
#16465=DIRECTION('',(1.,1.11022302462513E-14,0.));
#16466=DIRECTION('center_axis',(-1.0345260002189E-14,1.,0.));
#16467=DIRECTION('ref_axis',(-1.,-1.0345260002189E-14,0.));
#16468=DIRECTION('',(-1.,-1.11022302462516E-14,0.));
#16469=DIRECTION('',(1.,1.11022302462513E-14,0.));
#16470=DIRECTION('center_axis',(-1.0345260002189E-14,1.,0.));
#16471=DIRECTION('ref_axis',(-1.,-1.0345260002189E-14,0.));
#16472=DIRECTION('',(-1.,-1.11022302462516E-14,0.));
#16473=DIRECTION('',(1.,1.11022302462513E-14,0.));
#16474=DIRECTION('center_axis',(-1.0345260002189E-14,1.,0.));
#16475=DIRECTION('ref_axis',(-1.,-1.0345260002189E-14,0.));
#16476=DIRECTION('',(-1.,-1.11022302462516E-14,0.));
#16477=DIRECTION('',(1.,1.11022302462513E-14,0.));
#16478=DIRECTION('center_axis',(-1.0345260002189E-14,1.,0.));
#16479=DIRECTION('ref_axis',(-1.,-1.0345260002189E-14,0.));
#16480=DIRECTION('',(-1.,-1.11022302462516E-14,0.));
#16481=DIRECTION('center_axis',(0.,0.,-1.));
#16482=DIRECTION('ref_axis',(-1.,0.,0.));
#16483=DIRECTION('',(-1.0345260002189E-14,1.,0.));
#16484=DIRECTION('center_axis',(-1.0345260002189E-14,1.,0.));
#16485=DIRECTION('ref_axis',(1.,1.0345260002189E-14,-1.54206576648375E-14));
#16486=DIRECTION('',(-1.0345260002189E-14,1.,0.));
#16487=DIRECTION('center_axis',(0.,0.,1.));
#16488=DIRECTION('ref_axis',(1.,0.,0.));
#16489=DIRECTION('center_axis',(0.,0.,-1.));
#16490=DIRECTION('ref_axis',(-1.,0.,0.));
#16491=DIRECTION('',(-1.0345260002189E-14,1.,0.));
#16492=DIRECTION('center_axis',(-1.0345260002189E-14,1.,0.));
#16493=DIRECTION('ref_axis',(1.,1.0345260002189E-14,-3.43024899888577E-15));
#16494=DIRECTION('',(-1.0345260002189E-14,1.,0.));
#16495=DIRECTION('center_axis',(0.,0.,1.));
#16496=DIRECTION('ref_axis',(1.,0.,0.));
#16497=DIRECTION('center_axis',(0.,0.,-1.));
#16498=DIRECTION('ref_axis',(-1.,0.,0.));
#16499=DIRECTION('',(-1.0345260002189E-14,1.,0.));
#16500=DIRECTION('center_axis',(-1.0345260002189E-14,1.,0.));
#16501=DIRECTION('ref_axis',(1.,1.0345260002189E-14,-3.43024899888577E-15));
#16502=DIRECTION('',(-1.0345260002189E-14,1.,0.));
#16503=DIRECTION('center_axis',(0.,0.,1.));
#16504=DIRECTION('ref_axis',(1.,0.,0.));
#16505=DIRECTION('center_axis',(0.,0.,-1.));
#16506=DIRECTION('ref_axis',(-1.,0.,0.));
#16507=DIRECTION('',(-1.0345260002189E-14,1.,0.));
#16508=DIRECTION('center_axis',(-1.0345260002189E-14,1.,0.));
#16509=DIRECTION('ref_axis',(1.,1.0345260002189E-14,-1.54206576648375E-14));
#16510=DIRECTION('',(-1.0345260002189E-14,1.,0.));
#16511=DIRECTION('center_axis',(0.,0.,1.));
#16512=DIRECTION('ref_axis',(1.,0.,0.));
#16513=DIRECTION('center_axis',(0.707106781186551,7.34018225370516E-15,
-0.707106781186545));
#16514=DIRECTION('ref_axis',(1.03805852802452E-14,-1.,-1.32348907848756E-23));
#16515=DIRECTION('center_axis',(0.707106781186546,7.34018223498815E-15,
0.707106781186549));
#16516=DIRECTION('ref_axis',(1.03805852802452E-14,-1.,-1.32348895751129E-23));
#16517=DIRECTION('center_axis',(-0.707106781186546,-7.34018225370512E-15,
0.707106781186549));
#16518=DIRECTION('ref_axis',(1.03805852802452E-14,-1.,-1.3234889647637E-23));
#16519=DIRECTION('center_axis',(-0.707106781186544,-7.34018223498813E-15,
-0.707106781186551));
#16520=DIRECTION('ref_axis',(1.03805852802452E-14,-1.,-1.3234890851888E-23));
#16521=DIRECTION('center_axis',(0.,1.,-1.54886929424668E-30));
#16522=DIRECTION('ref_axis',(0.,1.54886929424668E-30,1.));
#16523=DIRECTION('center_axis',(-1.02244964895189E-14,1.,-1.57659325248097E-30));
#16524=DIRECTION('ref_axis',(-1.,-1.02244964895189E-14,1.11669963790763E-45));
#16525=DIRECTION('',(0.,1.,-1.54886929424668E-30));
#16526=DIRECTION('center_axis',(0.,1.,-1.54886929424668E-30));
#16527=DIRECTION('ref_axis',(0.,1.54886929424668E-30,1.));
#16528=DIRECTION('center_axis',(0.,1.,-1.54886929424668E-30));
#16529=DIRECTION('ref_axis',(0.,1.54886929424668E-30,1.));
#16530=DIRECTION('center_axis',(-1.02244964895189E-14,1.,-1.57659325248097E-30));
#16531=DIRECTION('ref_axis',(-1.,-1.02244964895189E-14,1.11669963790763E-45));
#16532=DIRECTION('',(0.,1.,-1.54886929424668E-30));
#16533=DIRECTION('center_axis',(0.,1.,-1.54886929424668E-30));
#16534=DIRECTION('ref_axis',(0.,1.54886929424668E-30,1.));
#16535=DIRECTION('center_axis',(1.,1.00583182218564E-14,1.5419764230905E-16));
#16536=DIRECTION('ref_axis',(-1.00583182218564E-14,1.,-8.58115691226271E-47));
#16537=DIRECTION('',(-7.00327082348719E-15,0.707106781186548,-0.707106781186548));
#16538=DIRECTION('',(1.5419764230905E-16,0.,-1.));
#16539=DIRECTION('',(7.2213392205266E-15,-0.707106781186548,-0.707106781186548));
#16540=DIRECTION('',(1.5419764230905E-16,0.,-1.));
#16541=DIRECTION('center_axis',(1.5419764230905E-16,1.,2.37769128936696E-32));
#16542=DIRECTION('ref_axis',(-1.,1.5419764230905E-16,0.));
#16543=DIRECTION('',(-1.,1.5419764230905E-16,-3.08395284618099E-16));
#16544=DIRECTION('',(1.5419764230905E-16,0.,-1.));
#16545=DIRECTION('',(1.,-1.5419764230905E-16,4.20834312723671E-32));
#16546=DIRECTION('center_axis',(1.5419764230905E-16,0.,-1.));
#16547=DIRECTION('ref_axis',(-1.,0.,-1.5419764230905E-16));
#16548=DIRECTION('center_axis',(1.35884999659177E-14,-0.707106781186556,
-0.70710678118654));
#16549=DIRECTION('ref_axis',(7.81974184165328E-13,0.70710678118654,-0.707106781186556));
#16550=DIRECTION('',(1.5419764230905E-16,0.,-1.));
#16551=DIRECTION('center_axis',(-3.88242856169051E-15,-0.707106781186542,
0.707106781186553));
#16552=DIRECTION('ref_axis',(1.03154041315431E-12,-0.707106781186553,-0.707106781186542));
#16553=DIRECTION('center_axis',(-0.986391978972164,0.164410656039619,-1.52099317550065E-16));
#16554=DIRECTION('ref_axis',(-0.164410656039619,-0.986391978972164,-3.75602913472012E-33));
#16555=DIRECTION('',(-0.117049568370783,-0.702246181386632,0.702246181386632));
#16556=DIRECTION('',(1.5419764230905E-16,0.,-1.));
#16557=DIRECTION('',(0.117049568370782,0.702246181386632,0.702246181386632));
#16558=DIRECTION('center_axis',(1.5419764230905E-16,0.,-1.));
#16559=DIRECTION('ref_axis',(-1.,0.,-1.5419764230905E-16));
#16560=DIRECTION('center_axis',(7.18968252164918E-15,0.707106781186545,
0.70710678118655));
#16561=DIRECTION('ref_axis',(7.1847046487102E-14,-0.70710678118655,0.707106781186545));
#16562=DIRECTION('',(1.5419764230905E-16,0.,-1.));
#16563=DIRECTION('center_axis',(2.93339046883292E-14,0.70710678118655,-0.707106781186545));
#16564=DIRECTION('ref_axis',(-2.48050675356169E-14,0.707106781186545,0.70710678118655));
#16565=DIRECTION('center_axis',(-1.02244964895189E-14,1.,-1.57659325248097E-30));
#16566=DIRECTION('ref_axis',(-1.,-1.02244964895189E-14,0.));
#16567=DIRECTION('',(-1.,-1.02244964895189E-14,1.00702988472098E-14));
#16568=DIRECTION('',(1.5419764230905E-16,0.,-1.));
#16569=DIRECTION('',(1.,1.02244964895189E-14,1.03786941318279E-14));
#16570=DIRECTION('center_axis',(1.5419764230905E-16,0.,-1.));
#16571=DIRECTION('ref_axis',(-1.,0.,-1.5419764230905E-16));
#16572=DIRECTION('center_axis',(7.90865077381428E-15,0.707106781186547,
0.707106781186548));
#16573=DIRECTION('ref_axis',(1.11137487371557E-13,-0.707106781186548,0.707106781186547));
#16574=DIRECTION('',(1.5419764230905E-16,0.,-1.));
#16575=DIRECTION('center_axis',(-1.4379365043298E-15,0.707106781186546,
-0.707106781186549));
#16576=DIRECTION('ref_axis',(1.95860265341088E-13,0.707106781186549,0.707106781186546));
#16577=DIRECTION('center_axis',(0.986391978972161,0.16441065603964,1.52099317550065E-16));
#16578=DIRECTION('ref_axis',(-0.16441065603964,0.986391978972161,2.47052149569693E-33));
#16579=DIRECTION('',(-0.117049568370797,0.702246181386631,-0.702246181386631));
#16580=DIRECTION('',(1.5419764230905E-16,0.,-1.));
#16581=DIRECTION('',(0.117049568370797,-0.702246181386631,-0.702246181386631));
#16582=DIRECTION('center_axis',(1.5419764230905E-16,0.,-1.));
#16583=DIRECTION('ref_axis',(-1.,0.,-1.5419764230905E-16));
#16584=DIRECTION('center_axis',(4.24155320364734E-14,-0.707106781186531,
-0.707106781186564));
#16585=DIRECTION('ref_axis',(-3.16030793522856E-12,0.707106781186564,-0.707106781186531));
#16586=DIRECTION('',(1.5419764230905E-16,0.,-1.));
#16587=DIRECTION('center_axis',(3.88242856169019E-15,-0.707106781186542,
0.707106781186553));
#16588=DIRECTION('ref_axis',(-2.80400082562096E-12,-0.707106781186553,-0.707106781186542));
#16589=DIRECTION('center_axis',(1.5419764230905E-16,1.,2.37769128936696E-32));
#16590=DIRECTION('ref_axis',(-1.,1.5419764230905E-16,0.));
#16591=DIRECTION('',(-1.,1.5419764230905E-16,-3.08395284618099E-16));
#16592=DIRECTION('',(1.5419764230905E-16,0.,-1.));
#16593=DIRECTION('',(1.,-1.5419764230905E-16,4.20834312723671E-32));
#16594=DIRECTION('center_axis',(-1.,-1.00583182218564E-14,-1.5419764230905E-16));
#16595=DIRECTION('ref_axis',(1.00583182218564E-14,-1.,8.58115691226271E-47));
#16596=DIRECTION('',(7.00327082348719E-15,-0.707106781186548,0.707106781186548));
#16597=DIRECTION('',(1.5419764230905E-16,0.,-1.));
#16598=DIRECTION('',(-7.2213392205266E-15,0.707106781186548,0.707106781186548));
#16599=DIRECTION('center_axis',(1.00447015340375E-14,-1.,1.54886929424668E-30));
#16600=DIRECTION('ref_axis',(1.,1.00447015340375E-14,0.));
#16601=DIRECTION('',(1.,1.00447015340375E-14,-9.89050389172848E-15));
#16602=DIRECTION('',(-1.,-1.00447015340375E-14,-1.01988991763466E-14));
#16603=DIRECTION('center_axis',(-1.09034198519707E-16,-0.707106781186547,
0.707106781186548));
#16604=DIRECTION('ref_axis',(2.24898714345845E-34,-0.707106781186548,-0.707106781186547));
#16605=DIRECTION('center_axis',(1.09034198519707E-16,-0.707106781186547,
-0.707106781186548));
#16606=DIRECTION('ref_axis',(-2.32788945572025E-33,0.707106781186548,-0.707106781186547));
#16607=DIRECTION('center_axis',(-2.46519032881566E-32,1.,-9.82547376793264E-15));
#16608=DIRECTION('ref_axis',(-1.41407071595279E-47,9.82547376793264E-15,
1.));
#16609=DIRECTION('center_axis',(2.7856650715617E-30,1.,1.00475183728577E-14));
#16610=DIRECTION('ref_axis',(-2.21644180929503E-45,-1.00475183728577E-14,
1.));
#16611=DIRECTION('',(-2.46519032881566E-32,1.,-9.82547376793264E-15));
#16612=DIRECTION('center_axis',(-2.46519032881566E-32,1.,-9.82547376793264E-15));
#16613=DIRECTION('ref_axis',(-1.41407071595279E-47,9.82547376793264E-15,
1.));
#16614=DIRECTION('center_axis',(-2.46519032881566E-32,1.,-9.82547376793264E-15));
#16615=DIRECTION('ref_axis',(-1.41407071595279E-47,9.82547376793264E-15,
1.));
#16616=DIRECTION('center_axis',(2.7856650715617E-30,1.,1.00475183728577E-14));
#16617=DIRECTION('ref_axis',(-2.21644180929503E-45,-1.00475183728577E-14,
1.));
#16618=DIRECTION('',(-2.46519032881566E-32,1.,-9.82547376793264E-15));
#16619=DIRECTION('center_axis',(-2.46519032881566E-32,1.,-9.82547376793264E-15));
#16620=DIRECTION('ref_axis',(-1.41407071595279E-47,9.82547376793264E-15,
1.));
#16621=DIRECTION('center_axis',(-2.71170936169723E-30,-1.,-9.82547376793264E-15));
#16622=DIRECTION('ref_axis',(0.,9.82547376793264E-15,-1.));
#16623=DIRECTION('',(3.13467930853623E-16,-9.82547376793264E-15,1.));
#16624=DIRECTION('',(-1.,2.715561221586E-32,2.77555756156289E-16));
#16625=DIRECTION('',(3.13467930853623E-16,-9.82547376793264E-15,1.));
#16626=DIRECTION('',(-1.,2.715561221586E-32,2.77555756156289E-16));
#16627=DIRECTION('center_axis',(-2.77555756156289E-16,-6.10622663543836E-16,
-1.));
#16628=DIRECTION('ref_axis',(-2.46519032881566E-32,1.,-6.10622663543836E-16));
#16629=DIRECTION('',(6.12323399573677E-17,-1.,6.10622663543836E-16));
#16630=DIRECTION('',(-1.,2.715561221586E-32,2.77555756156289E-16));
#16631=DIRECTION('',(6.12323399573677E-17,-1.,6.10622663543836E-16));
#16632=DIRECTION('center_axis',(-1.,2.715561221586E-32,2.77555756156289E-16));
#16633=DIRECTION('ref_axis',(2.77555756156289E-16,-7.53719648245999E-48,
1.));
#16634=DIRECTION('center_axis',(1.,6.12323399573675E-17,-3.13467930853623E-16));
#16635=DIRECTION('ref_axis',(3.13467930853623E-16,-1.43147286699433E-32,
1.));
#16636=DIRECTION('',(-1.,2.715561221586E-32,2.77555756156289E-16));
#16637=DIRECTION('center_axis',(1.,6.12323399573675E-17,-3.13467930853623E-16));
#16638=DIRECTION('ref_axis',(3.13467930853623E-16,1.91943749077616E-32,
1.));
#16639=DIRECTION('center_axis',(2.7856650715617E-30,1.,1.00475183728577E-14));
#16640=DIRECTION('ref_axis',(0.,-1.00475183728577E-14,1.));
#16641=DIRECTION('',(-3.13467930853624E-16,1.00475183728577E-14,-1.));
#16642=DIRECTION('',(-1.,2.715561221586E-32,2.77555756156289E-16));
#16643=DIRECTION('',(-3.13467930853624E-16,1.00475183728577E-14,-1.));
#16644=DIRECTION('center_axis',(-1.,2.715561221586E-32,2.77555756156289E-16));
#16645=DIRECTION('ref_axis',(2.77555756156289E-16,-7.53719648245999E-48,
1.));
#16646=DIRECTION('center_axis',(-1.,-6.12323399573675E-17,3.13467930853623E-16));
#16647=DIRECTION('ref_axis',(-3.13467930853623E-16,3.10928443355873E-33,
-1.));
#16648=DIRECTION('',(-1.,2.715561221586E-32,2.77555756156289E-16));
#16649=DIRECTION('center_axis',(-1.,-6.12323399573675E-17,3.13467930853623E-16));
#16650=DIRECTION('ref_axis',(-3.13467930853623E-16,-1.91943749077616E-32,
-1.));
#16651=DIRECTION('center_axis',(-2.77555756156289E-16,1.0991207943789E-14,
-1.));
#16652=DIRECTION('ref_axis',(-2.46519032881566E-32,1.,1.0991207943789E-14));
#16653=DIRECTION('',(6.1232339957364E-17,-1.,-1.0991207943789E-14));
#16654=DIRECTION('',(-1.,2.715561221586E-32,2.77555756156289E-16));
#16655=DIRECTION('',(6.1232339957364E-17,-1.,-1.0991207943789E-14));
#16656=DIRECTION('center_axis',(-1.,2.715561221586E-32,2.77555756156289E-16));
#16657=DIRECTION('ref_axis',(2.77555756156289E-16,-7.53719648245999E-48,
1.));
#16658=DIRECTION('center_axis',(1.,6.12323399573675E-17,-3.13467930853623E-16));
#16659=DIRECTION('ref_axis',(-3.13467930853623E-16,1.43147286699433E-32,
-1.));
#16660=DIRECTION('',(-1.,2.715561221586E-32,2.77555756156289E-16));
#16661=DIRECTION('center_axis',(1.,6.12323399573675E-17,-3.13467930853623E-16));
#16662=DIRECTION('ref_axis',(-3.13467930853623E-16,-1.91943749077616E-32,
-1.));
#16663=DIRECTION('center_axis',(-1.97215226305253E-31,1.,-6.10622663543836E-16));
#16664=DIRECTION('ref_axis',(-2.46519032881566E-32,6.10622663543836E-16,
1.));
#16665=DIRECTION('',(-3.13467930852236E-16,-6.10622663543836E-16,-1.));
#16666=DIRECTION('',(-1.,2.715561221586E-32,2.77555756156289E-16));
#16667=DIRECTION('',(-3.13467930852236E-16,-6.10622663543836E-16,-1.));
#16668=DIRECTION('center_axis',(2.77555756156289E-16,-1.02695629777827E-14,
1.));
#16669=DIRECTION('ref_axis',(2.46519032881566E-32,-1.,-1.02695629777827E-14));
#16670=DIRECTION('',(-6.12323399573645E-17,1.,1.02695629777827E-14));
#16671=DIRECTION('',(-6.12323399573645E-17,1.,1.02695629777827E-14));
#16672=DIRECTION('center_axis',(-1.,-6.12323399573675E-17,3.13467930853623E-16));
#16673=DIRECTION('ref_axis',(-3.13467930853623E-16,-6.10622663543836E-16,
-1.));
#16674=DIRECTION('center_axis',(-1.,-6.12323399573675E-17,3.13467930853623E-16));
#16675=DIRECTION('ref_axis',(-3.13467930853623E-16,-6.10622663543836E-16,
-1.));
#16676=DIRECTION('center_axis',(0.,1.,-9.82547376793264E-15));
#16677=DIRECTION('ref_axis',(0.,9.82547376793264E-15,1.));
#16678=DIRECTION('center_axis',(2.7856650715617E-30,1.,-1.01030295240889E-14));
#16679=DIRECTION('ref_axis',(2.37107728436212E-45,1.01030295240889E-14,
1.));
#16680=DIRECTION('',(0.,1.,-9.82547376793264E-15));
#16681=DIRECTION('center_axis',(0.,1.,-9.82547376793264E-15));
#16682=DIRECTION('ref_axis',(0.,9.82547376793264E-15,1.));
#16683=DIRECTION('center_axis',(0.,1.,-9.82547376793264E-15));
#16684=DIRECTION('ref_axis',(0.,9.82547376793264E-15,1.));
#16685=DIRECTION('center_axis',(2.7856650715617E-30,1.,-1.01030295240889E-14));
#16686=DIRECTION('ref_axis',(2.37107728436212E-45,1.01030295240889E-14,
1.));
#16687=DIRECTION('',(0.,1.,-9.82547376793264E-15));
#16688=DIRECTION('center_axis',(0.,1.,-9.82547376793264E-15));
#16689=DIRECTION('ref_axis',(0.,9.82547376793264E-15,1.));
#16690=DIRECTION('center_axis',(-2.71170936169723E-30,-1.,9.82547376793264E-15));
#16691=DIRECTION('ref_axis',(0.,9.82547376793264E-15,1.));
#16692=DIRECTION('',(3.13467930853623E-16,-9.82547376793264E-15,-1.));
#16693=DIRECTION('',(-1.,-8.66668474974256E-33,-2.77555756156289E-16));
#16694=DIRECTION('',(3.13467930853623E-16,-9.82547376793264E-15,-1.));
#16695=DIRECTION('',(-1.,-8.66668474974256E-33,-2.77555756156289E-16));
#16696=DIRECTION('center_axis',(-2.77555756156289E-16,-6.10622663543836E-16,
1.));
#16697=DIRECTION('ref_axis',(0.,1.,6.10622663543836E-16));
#16698=DIRECTION('',(6.12323399573677E-17,-1.,-6.10622663543836E-16));
#16699=DIRECTION('',(6.12323399573677E-17,-1.,-6.10622663543836E-16));
#16700=DIRECTION('',(-1.,-8.66668474974256E-33,-2.77555756156289E-16));
#16701=DIRECTION('center_axis',(-1.,-8.66668474974256E-33,-2.77555756156289E-16));
#16702=DIRECTION('ref_axis',(2.77555756156289E-16,2.40548823908298E-48,
-1.));
#16703=DIRECTION('center_axis',(-1.,-6.12323399573675E-17,-3.13467930853623E-16));
#16704=DIRECTION('ref_axis',(3.13467930853623E-16,-1.43147286699433E-32,
-1.));
#16705=DIRECTION('center_axis',(-1.,-6.12323399573675E-17,-3.13467930853623E-16));
#16706=DIRECTION('ref_axis',(3.13467930853623E-16,1.91943749077616E-32,
-1.));
#16707=DIRECTION('',(-1.,-8.66668474974256E-33,-2.77555756156289E-16));
#16708=DIRECTION('center_axis',(2.7856650715617E-30,1.,-1.01030295240889E-14));
#16709=DIRECTION('ref_axis',(2.46519032881566E-32,-1.01030295240889E-14,
-1.));
#16710=DIRECTION('',(-3.13467930853624E-16,1.01030295240889E-14,1.));
#16711=DIRECTION('',(-3.13467930853624E-16,1.01030295240889E-14,1.));
#16712=DIRECTION('',(-1.,-8.66668474974256E-33,-2.77555756156289E-16));
#16713=DIRECTION('center_axis',(-1.,-8.66668474974256E-33,-2.77555756156289E-16));
#16714=DIRECTION('ref_axis',(2.77555756156289E-16,2.40548823908298E-48,
-1.));
#16715=DIRECTION('center_axis',(1.,6.12323399573675E-17,3.13467930853623E-16));
#16716=DIRECTION('ref_axis',(-3.13467930853623E-16,3.10928443355873E-33,
1.));
#16717=DIRECTION('center_axis',(1.,6.12323399573675E-17,3.13467930853623E-16));
#16718=DIRECTION('ref_axis',(-3.13467930853623E-16,-1.91943749077616E-32,
1.));
#16719=DIRECTION('',(-1.,-8.66668474974256E-33,-2.77555756156289E-16));
#16720=DIRECTION('center_axis',(-2.77555756156289E-16,1.0991207943789E-14,
1.));
#16721=DIRECTION('ref_axis',(-2.46519032881566E-32,1.,-1.0991207943789E-14));
#16722=DIRECTION('',(6.1232339957364E-17,-1.,1.0991207943789E-14));
#16723=DIRECTION('',(6.1232339957364E-17,-1.,1.0991207943789E-14));
#16724=DIRECTION('',(-1.,-8.66668474974256E-33,-2.77555756156289E-16));
#16725=DIRECTION('center_axis',(-1.,-8.66668474974256E-33,-2.77555756156289E-16));
#16726=DIRECTION('ref_axis',(2.77555756156289E-16,2.40548823908298E-48,
-1.));
#16727=DIRECTION('center_axis',(-1.,-6.12323399573675E-17,-3.13467930853623E-16));
#16728=DIRECTION('ref_axis',(-3.13467930853623E-16,1.43147286699433E-32,
1.));
#16729=DIRECTION('center_axis',(-1.,-6.12323399573675E-17,-3.13467930853623E-16));
#16730=DIRECTION('ref_axis',(-3.13467930853623E-16,-1.91943749077616E-32,
1.));
#16731=DIRECTION('',(-1.,-8.66668474974256E-33,-2.77555756156289E-16));
#16732=DIRECTION('center_axis',(-1.72563323017096E-31,1.,6.10622663543836E-16));
#16733=DIRECTION('ref_axis',(4.86173068582901E-63,6.10622663543836E-16,
-1.));
#16734=DIRECTION('',(-3.13467930852236E-16,-6.10622663543836E-16,1.));
#16735=DIRECTION('',(-3.13467930852236E-16,-6.10622663543836E-16,1.));
#16736=DIRECTION('',(-1.,-8.66668474974256E-33,-2.77555756156289E-16));
#16737=DIRECTION('center_axis',(2.77555756156289E-16,-1.02695629777827E-14,
-1.));
#16738=DIRECTION('ref_axis',(0.,-1.,1.02695629777827E-14));
#16739=DIRECTION('',(-6.12323399573645E-17,1.,-1.02695629777827E-14));
#16740=DIRECTION('',(-6.12323399573645E-17,1.,-1.02695629777827E-14));
#16741=DIRECTION('center_axis',(-1.,-6.12323399573675E-17,-3.13467930853623E-16));
#16742=DIRECTION('ref_axis',(-3.13467930853623E-16,-6.10622663543836E-16,
1.));
#16743=DIRECTION('center_axis',(-1.,-6.12323399573675E-17,-3.13467930853623E-16));
#16744=DIRECTION('ref_axis',(-3.13467930853623E-16,-6.10622663543836E-16,
1.));
#16745=DIRECTION('',(-1.,-8.16511029819552E-17,-2.77555756156289E-17));
#16746=DIRECTION('',(-2.77555756156297E-17,9.72945507435399E-15,1.));
#16747=DIRECTION('',(-1.,-1.16360552223159E-15,-1.05243855142693E-15));
#16748=DIRECTION('',(-1.56697979189219E-15,0.707106781186538,0.707106781186557));
#16749=DIRECTION('',(-1.,-8.77500268227306E-17,-2.77555756156288E-16));
#16750=DIRECTION('',(-2.77555756156289E-16,8.95028523423949E-15,1.));
#16751=DIRECTION('',(0.,0.,1.));
#16752=DIRECTION('',(1.,0.,0.));
#16753=CARTESIAN_POINT('',(0.,0.,0.));
#16754=CARTESIAN_POINT('',(0.,0.,0.));
#16755=CARTESIAN_POINT('Origin',(0.,0.,115.));
#16756=CARTESIAN_POINT('',(160.,1.95943487863577E-14,-45.));
#16757=CARTESIAN_POINT('',(160.,-1.95943487863576E-14,-95.));
#16758=CARTESIAN_POINT('',(160.,-1.95943487863576E-14,115.));
#16759=CARTESIAN_POINT('',(56.5922444183314,149.657334840949,-95.));
#16760=CARTESIAN_POINT('Ctrl Pts',(56.5922444183314,149.657334840949,-95.));
#16761=CARTESIAN_POINT('Ctrl Pts',(60.5462378465639,148.162150106055,-95.));
#16762=CARTESIAN_POINT('Ctrl Pts',(64.4081265946212,146.52305102292,-94.8681994144769));
#16763=CARTESIAN_POINT('Ctrl Pts',(71.9578017024522,142.966730488755,-94.3871141013997));
#16764=CARTESIAN_POINT('Ctrl Pts',(75.6455459182189,141.049479319923,-94.0375811330598));
#16765=CARTESIAN_POINT('Ctrl Pts',(82.8520896158476,136.940627572589,-93.1507035872263));
#16766=CARTESIAN_POINT('Ctrl Pts',(86.3708709116552,134.74901877956,-92.6132279142068));
#16767=CARTESIAN_POINT('Ctrl Pts',(91.5232508355409,131.254717658139,-91.6807717500904));
#16768=CARTESIAN_POINT('Ctrl Pts',(93.2197161772174,130.055428691622,-91.3488437646329));
#16769=CARTESIAN_POINT('Ctrl Pts',(96.5704689047943,127.58712533728,-90.6445107692907));
#16770=CARTESIAN_POINT('Ctrl Pts',(98.2139345505394,126.326078432424,-90.2743825546963));
#16771=CARTESIAN_POINT('Ctrl Pts',(103.050070362074,122.465109833053,-89.1144758355367));
#16772=CARTESIAN_POINT('Ctrl Pts',(106.149349251733,119.786980782129,-88.2752185542421));
#16773=CARTESIAN_POINT('Ctrl Pts',(112.10933354305,114.228290909029,-86.4808050839628));
#16774=CARTESIAN_POINT('Ctrl Pts',(114.970003636752,111.347714259159,-85.5255886134343));
#16775=CARTESIAN_POINT('Ctrl Pts',(120.458203679568,105.386129890351,-83.5098605627197));
#16776=CARTESIAN_POINT('Ctrl Pts',(123.085719078493,102.305118804237,-82.4493145108988));
#16777=CARTESIAN_POINT('Ctrl Pts',(126.22481525846,98.3276308388503,-81.0620110399452));
#16778=CARTESIAN_POINT('Ctrl Pts',(126.845358313088,97.5258134181074,-80.7814609309442));
#16779=CARTESIAN_POINT('Ctrl Pts',(128.071857893764,95.9094803660136,-80.2142555183395));
#16780=CARTESIAN_POINT('Ctrl Pts',(128.677777212601,95.0949724534044,-79.9276008926568));
#16781=CARTESIAN_POINT('Ctrl Pts',(130.466680836712,92.6420084443857,-79.0620127301409));
#16782=CARTESIAN_POINT('Ctrl Pts',(131.623259690082,90.990947097925,-78.4763506491345));
#16783=CARTESIAN_POINT('Ctrl Pts',(137.230368463351,82.658242752523,-75.5075253594053));
#16784=CARTESIAN_POINT('Ctrl Pts',(141.156885196578,75.7456678635037,-73.0041701646379));
#16785=CARTESIAN_POINT('Ctrl Pts',(146.247760030425,65.0173884103724,-69.0861440470581));
#16786=CARTESIAN_POINT('Ctrl Pts',(147.810909187017,61.3811442891731,-67.7527018640001));
#16787=CARTESIAN_POINT('Ctrl Pts',(149.954354213166,55.8356435419837,-65.7130763478));
#16788=CARTESIAN_POINT('Ctrl Pts',(150.635252756495,53.9719392331638,-65.0266124141299));
#16789=CARTESIAN_POINT('Ctrl Pts',(151.605820654521,51.1533238711764,-63.9871451260196));
#16790=CARTESIAN_POINT('Ctrl Pts',(151.921076217439,50.2092866733786,-63.6387848556078));
#16791=CARTESIAN_POINT('Ctrl Pts',(152.532516926856,48.319945646416,-62.9412088896887));
#16792=CARTESIAN_POINT('Ctrl Pts',(152.828934942228,47.3740047564605,-62.5917585364604));
#16793=CARTESIAN_POINT('Ctrl Pts',(155.413776340098,38.8491671355886,-59.4409236358264));
#16794=CARTESIAN_POINT('Ctrl Pts',(157.125117056469,31.1910647608737,-56.5995154310153));
#16795=CARTESIAN_POINT('Ctrl Pts',(158.84500741576,19.5846841133227,-52.2866203497387));
#16796=CARTESIAN_POINT('Ctrl Pts',(159.276491887656,15.6959483595113,-50.8404415216121));
#16797=CARTESIAN_POINT('Ctrl Pts',(159.709623647027,9.83244782649476,-48.6590509514606));
#16798=CARTESIAN_POINT('Ctrl Pts',(159.818281747996,7.87287668664235,-47.9298972382464));
#16799=CARTESIAN_POINT('Ctrl Pts',(159.927179576913,4.92580700241418,-46.8331941701413));
#16800=CARTESIAN_POINT('Ctrl Pts',(159.968102560764,3.45034341369313,-46.2840992857951));
#16801=CARTESIAN_POINT('Ctrl Pts',(159.992025024361,1.72556508603403,-45.6421992563854));
#16802=CARTESIAN_POINT('Ctrl Pts',(159.997154300886,0.985641455265653,-45.3668240670506));
#16803=CARTESIAN_POINT('Ctrl Pts',(159.99943317645,0.492195768543,-45.1831795774147));
#16804=CARTESIAN_POINT('Ctrl Pts',(160.,0.244267011806123,-45.0909083946827));
#16805=CARTESIAN_POINT('Ctrl Pts',(160.,1.95943487863577E-14,-45.));
#16806=CARTESIAN_POINT('Origin',(0.,0.,-95.));
#16807=CARTESIAN_POINT('Origin',(0.,0.,-102.5));
#16808=CARTESIAN_POINT('',(170.,2.0818995585505E-14,-102.5));
#16809=CARTESIAN_POINT('',(-170.,-2.0818995585505E-14,-102.5));
#16810=CARTESIAN_POINT('Origin',(0.,0.,-102.5));
#16811=CARTESIAN_POINT('Origin',(0.,0.,-102.5));
#16812=CARTESIAN_POINT('',(-167.5,-2.05128338857182E-14,-105.));
#16813=CARTESIAN_POINT('Origin',(-167.5,-2.05128338857182E-14,-102.5));
#16814=CARTESIAN_POINT('Origin',(0.,0.,-105.));
#16815=CARTESIAN_POINT('Origin',(121.449578014911,-122.5,115.));
#16816=CARTESIAN_POINT('',(121.449578014911,-125.,32.5));
#16817=CARTESIAN_POINT('',(119.689439203101,-120.724637681159,32.5));
#16818=CARTESIAN_POINT('Origin',(121.449578014911,-122.5,32.5));
#16819=CARTESIAN_POINT('',(121.449578014911,-125.,-32.5));
#16820=CARTESIAN_POINT('',(121.449578014911,-125.,85.));
#16821=CARTESIAN_POINT('',(119.689439203101,-120.724637681159,-32.5));
#16822=CARTESIAN_POINT('Origin',(121.449578014911,-122.5,-32.5));
#16823=CARTESIAN_POINT('',(119.689439203101,-120.724637681159,115.));
#16824=CARTESIAN_POINT('Origin',(121.449578014911,-122.5,115.));
#16825=CARTESIAN_POINT('',(119.689439203101,-120.724637681159,82.5));
#16826=CARTESIAN_POINT('',(118.949578014911,-122.5,82.5));
#16827=CARTESIAN_POINT('Origin',(121.449578014911,-122.5,82.5));
#16828=CARTESIAN_POINT('',(121.449578014911,-125.,82.5));
#16829=CARTESIAN_POINT('Origin',(121.449578014911,-122.5,82.5));
#16830=CARTESIAN_POINT('',(121.449578014911,-125.,49.5));
#16831=CARTESIAN_POINT('',(121.449578014911,-125.,85.));
#16832=CARTESIAN_POINT('',(119.689439203101,-120.724637681159,49.5));
#16833=CARTESIAN_POINT('Origin',(121.449578014911,-122.5,49.5));
#16834=CARTESIAN_POINT('',(119.689439203101,-120.724637681159,115.));
#16835=CARTESIAN_POINT('Origin',(121.449578014911,-122.5,115.));
#16836=CARTESIAN_POINT('',(121.449578014911,-125.,-49.5));
#16837=CARTESIAN_POINT('',(119.689439203101,-120.724637681159,-49.5));
#16838=CARTESIAN_POINT('Origin',(121.449578014911,-122.5,-49.5));
#16839=CARTESIAN_POINT('',(121.449578014911,-125.,-82.5));
#16840=CARTESIAN_POINT('',(121.449578014911,-125.,85.));
#16841=CARTESIAN_POINT('',(119.689439203101,-120.724637681159,-82.5));
#16842=CARTESIAN_POINT('Origin',(121.449578014911,-122.5,-82.5));
#16843=CARTESIAN_POINT('',(119.689439203101,-120.724637681159,115.));
#16844=CARTESIAN_POINT('Origin',(-121.449578014911,-122.5,49.5));
#16845=CARTESIAN_POINT('',(-121.449578014911,-122.5,47.));
#16846=CARTESIAN_POINT('',(-119.689439203101,-120.724637681159,49.5));
#16847=CARTESIAN_POINT('Origin',(-121.449578014911,-122.5,49.5));
#16848=CARTESIAN_POINT('',(-121.449578014911,-125.,49.5));
#16849=CARTESIAN_POINT('Origin',(-121.449578014911,-122.5,49.5));
#16850=CARTESIAN_POINT('Origin',(-121.449578014911,-122.5,49.5));
#16851=CARTESIAN_POINT('Origin',(-121.449578014911,-122.5,32.5));
#16852=CARTESIAN_POINT('',(-119.689439203101,-120.724637681159,32.5));
#16853=CARTESIAN_POINT('',(-121.449578014911,-125.,32.5));
#16854=CARTESIAN_POINT('Origin',(-121.449578014911,-122.5,32.5));
#16855=CARTESIAN_POINT('',(-121.449578014911,-122.5,35.));
#16856=CARTESIAN_POINT('Origin',(-121.449578014911,-122.5,32.5));
#16857=CARTESIAN_POINT('Origin',(-121.449578014911,-122.5,32.5));
#16858=CARTESIAN_POINT('Origin',(-121.449578014911,-122.5,-32.5));
#16859=CARTESIAN_POINT('',(-119.689439203101,-120.724637681159,-32.5));
#16860=CARTESIAN_POINT('',(-121.449578014911,-122.5,-35.));
#16861=CARTESIAN_POINT('Origin',(-121.449578014911,-122.5,-32.5));
#16862=CARTESIAN_POINT('',(-121.449578014911,-125.,-32.5));
#16863=CARTESIAN_POINT('Origin',(-121.449578014911,-122.5,-32.5));
#16864=CARTESIAN_POINT('Origin',(-121.449578014911,-122.5,-32.5));
#16865=CARTESIAN_POINT('Origin',(-121.449578014911,-122.5,-49.5));
#16866=CARTESIAN_POINT('',(-121.449578014911,-125.,-49.5));
#16867=CARTESIAN_POINT('',(-119.689439203101,-120.724637681159,-49.5));
#16868=CARTESIAN_POINT('Origin',(-121.449578014911,-122.5,-49.5));
#16869=CARTESIAN_POINT('',(-121.449578014911,-122.5,-47.));
#16870=CARTESIAN_POINT('Origin',(-121.449578014911,-122.5,-49.5));
#16871=CARTESIAN_POINT('Origin',(-121.449578014911,-122.5,-49.5));
#16872=CARTESIAN_POINT('Origin',(0.,0.,124.));
#16873=CARTESIAN_POINT('',(-194.,-2.37581479034587E-14,125.));
#16874=CARTESIAN_POINT('Origin',(0.,0.,125.));
#16875=CARTESIAN_POINT('',(-195.,-2.38806125833734E-14,124.));
#16876=CARTESIAN_POINT('Origin',(-194.,-2.37581479034587E-14,124.));
#16877=CARTESIAN_POINT('',(195.,2.38806125833734E-14,124.));
#16878=CARTESIAN_POINT('Origin',(0.,0.,124.));
#16879=CARTESIAN_POINT('Origin',(0.,0.,124.));
#16880=CARTESIAN_POINT('Origin',(0.,0.,116.));
#16881=CARTESIAN_POINT('',(195.,2.38806125833734E-14,116.));
#16882=CARTESIAN_POINT('',(-195.,-2.38806125833734E-14,116.));
#16883=CARTESIAN_POINT('Origin',(0.,0.,116.));
#16884=CARTESIAN_POINT('Origin',(0.,0.,116.));
#16885=CARTESIAN_POINT('',(-194.,-2.37581479034587E-14,115.));
#16886=CARTESIAN_POINT('Origin',(-194.,-2.37581479034587E-14,116.));
#16887=CARTESIAN_POINT('Origin',(0.,0.,115.));
#16888=CARTESIAN_POINT('Origin',(155.884572681198,90.0000000000018,125.));
#16889=CARTESIAN_POINT('',(151.384572681198,90.0000000000018,124.475));
#16890=CARTESIAN_POINT('Origin',(155.884572681198,90.0000000000018,124.475));
#16891=CARTESIAN_POINT('',(150.859572681198,90.0000000000018,125.));
#16892=CARTESIAN_POINT('',(150.859572681198,90.0000000000018,125.));
#16893=CARTESIAN_POINT('Origin',(155.884572681198,90.0000000000018,125.));
#16894=CARTESIAN_POINT('Origin',(155.884572681198,90.0000000000018,125.));
#16895=CARTESIAN_POINT('',(151.384572681198,90.0000000000018,115.));
#16896=CARTESIAN_POINT('Origin',(155.884572681198,90.0000000000018,115.));
#16897=CARTESIAN_POINT('',(151.384572681198,90.0000000000018,125.));
#16898=CARTESIAN_POINT('Origin',(155.8845726812,-89.9999999999986,125.));
#16899=CARTESIAN_POINT('',(151.3845726812,-89.9999999999986,124.475));
#16900=CARTESIAN_POINT('Origin',(155.8845726812,-89.9999999999986,124.475));
#16901=CARTESIAN_POINT('',(150.8595726812,-89.9999999999986,125.));
#16902=CARTESIAN_POINT('',(150.8595726812,-89.9999999999986,125.));
#16903=CARTESIAN_POINT('Origin',(155.8845726812,-89.9999999999986,125.));
#16904=CARTESIAN_POINT('Origin',(155.8845726812,-89.9999999999986,125.));
#16905=CARTESIAN_POINT('',(151.3845726812,-89.9999999999986,115.));
#16906=CARTESIAN_POINT('Origin',(155.8845726812,-89.9999999999986,115.));
#16907=CARTESIAN_POINT('',(151.3845726812,-89.9999999999986,125.));
#16908=CARTESIAN_POINT('Origin',(0.,-180.,125.));
#16909=CARTESIAN_POINT('',(-4.49999999999999,-180.,124.475));
#16910=CARTESIAN_POINT('Origin',(0.,-180.,124.475));
#16911=CARTESIAN_POINT('',(-5.025,-180.,125.));
#16912=CARTESIAN_POINT('',(-5.025,-180.,125.));
#16913=CARTESIAN_POINT('Origin',(0.,-180.,125.));
#16914=CARTESIAN_POINT('Origin',(0.,-180.,125.));
#16915=CARTESIAN_POINT('',(-4.49999999999998,-180.,115.));
#16916=CARTESIAN_POINT('Origin',(0.,-180.,115.));
#16917=CARTESIAN_POINT('',(-4.49999999999998,-180.,125.));
#16918=CARTESIAN_POINT('Origin',(-155.884572681199,-90.0000000000007,125.));
#16919=CARTESIAN_POINT('',(-160.384572681199,-90.0000000000007,124.475));
#16920=CARTESIAN_POINT('Origin',(-155.884572681199,-90.0000000000007,124.475));
#16921=CARTESIAN_POINT('',(-160.909572681199,-90.0000000000007,125.));
#16922=CARTESIAN_POINT('',(-160.909572681199,-90.0000000000007,125.));
#16923=CARTESIAN_POINT('Origin',(-155.884572681199,-90.0000000000007,125.));
#16924=CARTESIAN_POINT('Origin',(-155.884572681199,-90.0000000000007,125.));
#16925=CARTESIAN_POINT('',(-160.384572681199,-90.0000000000007,115.));
#16926=CARTESIAN_POINT('Origin',(-155.884572681199,-90.0000000000007,115.));
#16927=CARTESIAN_POINT('',(-160.384572681199,-90.0000000000007,125.));
#16928=CARTESIAN_POINT('Origin',(-155.884572681199,89.9999999999996,125.));
#16929=CARTESIAN_POINT('',(-160.384572681199,89.9999999999996,124.475));
#16930=CARTESIAN_POINT('Origin',(-155.884572681199,89.9999999999996,124.475));
#16931=CARTESIAN_POINT('',(-160.909572681199,89.9999999999996,125.));
#16932=CARTESIAN_POINT('',(-160.909572681199,89.9999999999996,125.));
#16933=CARTESIAN_POINT('Origin',(-155.884572681199,89.9999999999996,125.));
#16934=CARTESIAN_POINT('Origin',(-155.884572681199,89.9999999999996,125.));
#16935=CARTESIAN_POINT('',(-160.384572681199,89.9999999999996,115.));
#16936=CARTESIAN_POINT('Origin',(-155.884572681199,89.9999999999996,115.));
#16937=CARTESIAN_POINT('',(-160.384572681199,89.9999999999996,125.));
#16938=CARTESIAN_POINT('Origin',(0.,180.,125.));
#16939=CARTESIAN_POINT('',(-4.49999999999999,180.,124.475));
#16940=CARTESIAN_POINT('Origin',(0.,180.,124.475));
#16941=CARTESIAN_POINT('',(-5.025,180.,125.));
#16942=CARTESIAN_POINT('',(-5.025,180.,125.));
#16943=CARTESIAN_POINT('Origin',(0.,180.,125.));
#16944=CARTESIAN_POINT('Origin',(0.,180.,125.));
#16945=CARTESIAN_POINT('',(-4.49999999999998,180.,115.));
#16946=CARTESIAN_POINT('Origin',(0.,180.,115.));
#16947=CARTESIAN_POINT('',(-4.49999999999998,180.,125.));
#16948=CARTESIAN_POINT('Origin',(0.,0.,125.));
#16949=CARTESIAN_POINT('',(195.,-2.38806125833734E-14,125.));
#16950=CARTESIAN_POINT('Origin',(0.,0.,-103.));
#16951=CARTESIAN_POINT('',(35.5,-4.3474961369731E-15,-103.));
#16952=CARTESIAN_POINT('Origin',(0.,0.,-103.));
#16953=CARTESIAN_POINT('',(37.5,-4.59242549680257E-15,-105.));
#16954=CARTESIAN_POINT('',(35.5,-4.3474961369731E-15,-103.));
#16955=CARTESIAN_POINT('Origin',(0.,0.,-105.));
#16956=CARTESIAN_POINT('Origin',(0.,0.,-96.9999999999999));
#16957=CARTESIAN_POINT('',(35.5,4.3474961369731E-15,-96.9999999999999));
#16958=CARTESIAN_POINT('',(-35.5,-4.3474961369731E-15,-96.9999999999999));
#16959=CARTESIAN_POINT('Origin',(0.,0.,-96.9999999999999));
#16960=CARTESIAN_POINT('Origin',(0.,0.,-96.9999999999999));
#16961=CARTESIAN_POINT('',(-37.5,-4.59242549680257E-15,-95.));
#16962=CARTESIAN_POINT('',(-35.5,-4.3474961369731E-15,-96.9999999999999));
#16963=CARTESIAN_POINT('Origin',(0.,0.,-95.));
#16964=CARTESIAN_POINT('Origin',(0.,0.,-93.));
#16965=CARTESIAN_POINT('',(35.5,-4.3474961369731E-15,-93.));
#16966=CARTESIAN_POINT('Origin',(-169.,-140.,-65.));
#16967=CARTESIAN_POINT('',(-169.,-125.,-60.5));
#16968=CARTESIAN_POINT('Origin',(-169.,-125.,-65.));
#16969=CARTESIAN_POINT('',(-169.,-140.,-60.5));
#16970=CARTESIAN_POINT('',(-169.,-140.,-60.5));
#16971=CARTESIAN_POINT('Origin',(-169.,-140.,-65.));
#16972=CARTESIAN_POINT('Origin',(-169.,-140.,65.));
#16973=CARTESIAN_POINT('',(-169.,-125.,69.5));
#16974=CARTESIAN_POINT('Origin',(-169.,-125.,65.));
#16975=CARTESIAN_POINT('',(-169.,-140.,69.5));
#16976=CARTESIAN_POINT('',(-169.,-140.,69.5));
#16977=CARTESIAN_POINT('Origin',(-169.,-140.,65.));
#16978=CARTESIAN_POINT('Origin',(169.,-140.,-65.));
#16979=CARTESIAN_POINT('',(169.,-125.,-60.5));
#16980=CARTESIAN_POINT('Origin',(169.,-125.,-65.));
#16981=CARTESIAN_POINT('',(169.,-140.,-60.5));
#16982=CARTESIAN_POINT('',(169.,-140.,-60.5));
#16983=CARTESIAN_POINT('Origin',(169.,-140.,-65.));
#16984=CARTESIAN_POINT('Origin',(169.,-140.,65.));
#16985=CARTESIAN_POINT('',(169.,-125.,69.5));
#16986=CARTESIAN_POINT('Origin',(169.,-125.,65.));
#16987=CARTESIAN_POINT('',(169.,-140.,69.5));
#16988=CARTESIAN_POINT('',(169.,-140.,69.5));
#16989=CARTESIAN_POINT('Origin',(169.,-140.,65.));
#16990=CARTESIAN_POINT('Origin',(-95.,158.745078663875,115.));
#16991=CARTESIAN_POINT('',(-82.1621621621622,137.293041006595,-44.9999999999999));
#16992=CARTESIAN_POINT('',(-91.875,183.548997205106,-45.));
#16993=CARTESIAN_POINT('Origin',(-95.,158.745078663875,-45.));
#16994=CARTESIAN_POINT('',(-91.875,183.548997205106,45.0000000000001));
#16995=CARTESIAN_POINT('',(-91.875,183.548997205106,-105.));
#16996=CARTESIAN_POINT('',(-82.1621621621622,137.293041006595,45.0000000000001));
#16997=CARTESIAN_POINT('Origin',(-95.,158.745078663875,45.0000000000001));
#16998=CARTESIAN_POINT('',(-82.1621621621621,137.293041006595,115.));
#16999=CARTESIAN_POINT('Origin',(0.,0.,115.));
#17000=CARTESIAN_POINT('',(-12.5969447708578,159.503344737469,-95.));
#17001=CARTESIAN_POINT('Origin',(0.,0.,-95.));
#17002=CARTESIAN_POINT('Ctrl Pts',(-82.1621621621622,137.293041006595,-45.));
#17003=CARTESIAN_POINT('Ctrl Pts',(-82.1621621620898,137.293041006638,-45.8956808810957));
#17004=CARTESIAN_POINT('Ctrl Pts',(-82.1332503382887,137.310362174487,-46.7855749735046));
#17005=CARTESIAN_POINT('Ctrl Pts',(-82.0763076034376,137.344386309753,-47.6698671589124));
#17006=CARTESIAN_POINT('Ctrl Pts',(-82.0604557369373,137.353858036944,-47.9160387154245));
#17007=CARTESIAN_POINT('Ctrl Pts',(-82.042431814488,137.36462402734,-48.161776221576));
#17008=CARTESIAN_POINT('Ctrl Pts',(-82.0222554199955,137.376670566071,-48.4070838498355));
#17009=CARTESIAN_POINT('Ctrl Pts',(-81.9465407866535,137.421876822489,-49.3276337100496));
#17010=CARTESIAN_POINT('Ctrl Pts',(-81.840502580685,137.485121623027,-50.2421320047361));
#17011=CARTESIAN_POINT('Ctrl Pts',(-81.7046585719633,137.56579962954,-51.1506976196694));
#17012=CARTESIAN_POINT('Ctrl Pts',(-81.6751455849419,137.583327446788,-51.3480893593125));
#17013=CARTESIAN_POINT('Ctrl Pts',(-81.6442279669171,137.601676775247,-51.5451821462862));
#17014=CARTESIAN_POINT('Ctrl Pts',(-81.6119109575879,137.620841408021,-51.7419836113765));
#17015=CARTESIAN_POINT('Ctrl Pts',(-81.497776835662,137.688525224661,-52.4370281986711));
#17016=CARTESIAN_POINT('Ctrl Pts',(-81.3661884614961,137.766377965718,-53.1284391494042));
#17017=CARTESIAN_POINT('Ctrl Pts',(-81.2171404377993,137.854188085092,-53.8164994257697));
#17018=CARTESIAN_POINT('Ctrl Pts',(-81.1308907209676,137.905001223993,-54.2146597134931));
#17019=CARTESIAN_POINT('Ctrl Pts',(-81.0387936079803,137.959149117421,-54.6116977958882));
#17020=CARTESIAN_POINT('Ctrl Pts',(-80.9408410263292,138.01659412532,-55.0076668915174));
#17021=CARTESIAN_POINT('Ctrl Pts',(-80.8078101077321,138.094611080472,-55.5454386545451));
#17022=CARTESIAN_POINT('Ctrl Pts',(-80.6639677088331,138.178711759688,-56.0812362030082));
#17023=CARTESIAN_POINT('Ctrl Pts',(-80.5092092471911,138.268822322297,-56.6151741291791));
#17024=CARTESIAN_POINT('Ctrl Pts',(-80.4598920531534,138.297538038736,-56.7853252151335));
#17025=CARTESIAN_POINT('Ctrl Pts',(-80.4094775869982,138.326857136585,-56.955221756991));
#17026=CARTESIAN_POINT('Ctrl Pts',(-80.3580264160791,138.356740035565,-57.1246996088993));
#17027=CARTESIAN_POINT('Ctrl Pts',(-80.2486201865606,138.420283298937,-57.48507882735));
#17028=CARTESIAN_POINT('Ctrl Pts',(-80.1344832799705,138.486400947608,-57.8436980583636));
#17029=CARTESIAN_POINT('Ctrl Pts',(-80.0161972390454,138.55471186287,-58.1989404973028));
#17030=CARTESIAN_POINT('Ctrl Pts',(-79.7044269738313,138.734761106227,-59.1352642472327));
#17031=CARTESIAN_POINT('Ctrl Pts',(-79.3625347898603,138.930810670846,-60.0529663482358));
#17032=CARTESIAN_POINT('Ctrl Pts',(-78.9916175899106,139.141382683262,-60.9537945777502));
#17033=CARTESIAN_POINT('Ctrl Pts',(-78.9517483894941,139.164016677497,-61.0506229298144));
#17034=CARTESIAN_POINT('Ctrl Pts',(-78.9115438397022,139.186818412233,-61.1472563431337));
#17035=CARTESIAN_POINT('Ctrl Pts',(-78.8710053024311,139.209786015874,-61.2436970022178));
#17036=CARTESIAN_POINT('Ctrl Pts',(-78.653076104096,139.333256466116,-61.762147763787));
#17037=CARTESIAN_POINT('Ctrl Pts',(-78.4254901802515,139.461523555169,-62.2750241275225));
#17038=CARTESIAN_POINT('Ctrl Pts',(-78.1883402386737,139.594353793634,-62.7825737116347));
#17039=CARTESIAN_POINT('Ctrl Pts',(-77.9757260681242,139.71344128228,-63.2376117062502));
#17040=CARTESIAN_POINT('Ctrl Pts',(-77.7554805786764,139.836164959048,-63.6882429907043));
#17041=CARTESIAN_POINT('Ctrl Pts',(-77.5277216033442,139.962324869928,-64.1345780407656));
#17042=CARTESIAN_POINT('Ctrl Pts',(-77.3016103965922,140.087572051301,-64.5776839892267));
#17043=CARTESIAN_POINT('Ctrl Pts',(-77.0680917138838,140.216207282072,-65.0165537711084));
#17044=CARTESIAN_POINT('Ctrl Pts',(-76.8272244703531,140.348059230023,-65.4512527482325));
#17045=CARTESIAN_POINT('Ctrl Pts',(-76.5598938718774,140.494397352381,-65.9337107861455));
#17046=CARTESIAN_POINT('Ctrl Pts',(-76.283495691648,140.6447064215,-66.4110683238974));
#17047=CARTESIAN_POINT('Ctrl Pts',(-75.9981293972275,140.798736954998,-66.8833902572378));
#17048=CARTESIAN_POINT('Ctrl Pts',(-75.7822524315751,140.915259630728,-67.2406974367265));
#17049=CARTESIAN_POINT('Ctrl Pts',(-75.5610017760309,141.034037807636,-67.5954458574455));
#17050=CARTESIAN_POINT('Ctrl Pts',(-75.3356990939032,141.154285467157,-67.9457481010467));
#17051=CARTESIAN_POINT('Ctrl Pts',(-75.3201844290252,141.162565892948,-67.9698704144792));
#17052=CARTESIAN_POINT('Ctrl Pts',(-75.3046505622078,141.170853279768,-67.9939716299542));
#17053=CARTESIAN_POINT('Ctrl Pts',(-75.2890979304666,141.179147367824,-68.0180511247126));
#17054=CARTESIAN_POINT('Ctrl Pts',(-75.248703999487,141.200689112399,-68.080591372915));
#17055=CARTESIAN_POINT('Ctrl Pts',(-75.2081802678764,141.222277777914,-68.1429904246721));
#17056=CARTESIAN_POINT('Ctrl Pts',(-75.1675344072028,141.243908793063,-68.205237202427));
#17057=CARTESIAN_POINT('Ctrl Pts',(-74.8854046764752,141.394053294326,-68.6373025186886));
#17058=CARTESIAN_POINT('Ctrl Pts',(-74.5969543424691,141.546476593965,-69.0627940644927));
#17059=CARTESIAN_POINT('Ctrl Pts',(-74.3023794330922,141.700940048339,-69.4819598157056));
#17060=CARTESIAN_POINT('Ctrl Pts',(-73.9413538470785,141.890247614456,-69.9956816438427));
#17061=CARTESIAN_POINT('Ctrl Pts',(-73.5711387365508,142.082613055927,-70.4999175422413));
#17062=CARTESIAN_POINT('Ctrl Pts',(-73.1920302731841,142.277638576512,-70.9950211945631));
#17063=CARTESIAN_POINT('Ctrl Pts',(-72.9571177373819,142.398485099378,-71.3018095300674));
#17064=CARTESIAN_POINT('Ctrl Pts',(-72.7187910465147,142.520352610966,-71.6050922936546));
#17065=CARTESIAN_POINT('Ctrl Pts',(-72.4771257062136,142.643143015591,-71.904961551415));
#17066=CARTESIAN_POINT('Ctrl Pts',(-72.2471941166274,142.759971489571,-72.1902710418823));
#17067=CARTESIAN_POINT('Ctrl Pts',(-72.0142391557779,142.877636119185,-72.472488769632));
#17068=CARTESIAN_POINT('Ctrl Pts',(-71.7783094935174,142.996063179386,-72.751667986971));
#17069=CARTESIAN_POINT('Ctrl Pts',(-71.3719031956286,143.200062552101,-73.2325748431889));
#17070=CARTESIAN_POINT('Ctrl Pts',(-70.9566250939629,143.406347242988,-73.7045023042245));
#17071=CARTESIAN_POINT('Ctrl Pts',(-70.5326862235245,143.614554186242,-74.1678187118353));
#17072=CARTESIAN_POINT('Ctrl Pts',(-70.0130610572177,143.869755053769,-74.7357092313069));
#17073=CARTESIAN_POINT('Ctrl Pts',(-69.4804552925272,144.127824642797,-75.2907111591283));
#17074=CARTESIAN_POINT('Ctrl Pts',(-68.9350883593252,144.388196564031,-75.8332462671249));
#17075=CARTESIAN_POINT('Ctrl Pts',(-68.5485065908993,144.572760445027,-76.2178207044695));
#17076=CARTESIAN_POINT('Ctrl Pts',(-68.1555132304399,144.758480717796,-76.596131950207));
#17077=CARTESIAN_POINT('Ctrl Pts',(-67.7561927121406,144.945149385449,-76.9683433312052));
#17078=CARTESIAN_POINT('Ctrl Pts',(-67.2837105909669,145.166018597041,-77.4087495080978));
#17079=CARTESIAN_POINT('Ctrl Pts',(-66.8023415189655,145.388228815956,-77.8406036136869));
#17080=CARTESIAN_POINT('Ctrl Pts',(-66.3123287087178,145.611383693817,-78.2640873513956));
#17081=CARTESIAN_POINT('Ctrl Pts',(-66.0648257909633,145.724098060108,-78.4779867811913));
#17082=CARTESIAN_POINT('Ctrl Pts',(-65.8148876609796,145.837153384037,-78.6899061289426));
#17083=CARTESIAN_POINT('Ctrl Pts',(-65.5628580637272,145.950365739295,-78.8996153026583));
#17084=CARTESIAN_POINT('Ctrl Pts',(-65.1942221791109,146.115957944278,-79.206350414755));
#17085=CARTESIAN_POINT('Ctrl Pts',(-64.820779748259,146.282034503608,-79.5086408854622));
#17086=CARTESIAN_POINT('Ctrl Pts',(-64.4438701328714,146.447897285852,-79.8055427686403));
#17087=CARTESIAN_POINT('Ctrl Pts',(-64.3122652712965,146.505811299202,-79.9092114723342));
#17088=CARTESIAN_POINT('Ctrl Pts',(-64.1802381240679,146.56369914227,-80.0122234022978));
#17089=CARTESIAN_POINT('Ctrl Pts',(-64.0478469452313,146.621530825729,-80.1145390866013));
#17090=CARTESIAN_POINT('Ctrl Pts',(-63.78695174754,146.735496186726,-80.3161663469507));
#17091=CARTESIAN_POINT('Ctrl Pts',(-63.5245936249025,146.849270772549,-80.5151564102869));
#17092=CARTESIAN_POINT('Ctrl Pts',(-63.2608931848606,146.962781832294,-80.7114996909868));
#17093=CARTESIAN_POINT('Ctrl Pts',(-62.7500940644695,147.182657648439,-81.0918250899897));
#17094=CARTESIAN_POINT('Ctrl Pts',(-62.2338700369337,147.401712680234,-81.4625003839186));
#17095=CARTESIAN_POINT('Ctrl Pts',(-61.7123790491669,147.619721826396,-81.8239969669797));
#17096=CARTESIAN_POINT('Ctrl Pts',(-60.9875045505543,147.922755386369,-82.3264786215886));
#17097=CARTESIAN_POINT('Ctrl Pts',(-60.2524717621619,148.22375568285,-82.8112825188533));
#17098=CARTESIAN_POINT('Ctrl Pts',(-59.5075864500793,148.522204166141,-83.2793071779857));
#17099=CARTESIAN_POINT('Ctrl Pts',(-59.1501577232241,148.665412871809,-83.5038859894309));
#17100=CARTESIAN_POINT('Ctrl Pts',(-58.7904606523049,148.808033919482,-83.724602128888));
#17101=CARTESIAN_POINT('Ctrl Pts',(-58.4285301239598,148.950009475213,-83.9415589199558));
#17102=CARTESIAN_POINT('Ctrl Pts',(-57.911059102069,149.152999359055,-84.2517534009057));
#17103=CARTESIAN_POINT('Ctrl Pts',(-57.3890213558604,149.354670232681,-84.5542415763276));
#17104=CARTESIAN_POINT('Ctrl Pts',(-56.8625067494514,149.554857247062,-84.8493362502414));
#17105=CARTESIAN_POINT('Ctrl Pts',(-55.9822840681341,149.889528210448,-85.3426730389139));
#17106=CARTESIAN_POINT('Ctrl Pts',(-55.0895386431195,150.220060731732,-85.8153114005049));
#17107=CARTESIAN_POINT('Ctrl Pts',(-54.1845193914356,150.545796080153,-86.2681831732401));
#17108=CARTESIAN_POINT('Ctrl Pts',(-53.3953903177273,150.829820130796,-86.6630634830924));
#17109=CARTESIAN_POINT('Ctrl Pts',(-52.5969297863791,151.110196736556,-87.0429162429449));
#17110=CARTESIAN_POINT('Ctrl Pts',(-51.7893118661202,151.386482806261,-87.4083895500494));
#17111=CARTESIAN_POINT('Ctrl Pts',(-50.7892348830617,151.72860911639,-87.8609568262193));
#17112=CARTESIAN_POINT('Ctrl Pts',(-49.7751097566078,152.064469149807,-88.2914533321514));
#17113=CARTESIAN_POINT('Ctrl Pts',(-48.7471190027564,152.393300182218,-88.7006682117858));
#17114=CARTESIAN_POINT('Ctrl Pts',(-48.4756335577533,152.480142246537,-88.8087391095864));
#17115=CARTESIAN_POINT('Ctrl Pts',(-48.2031811311436,152.566494018159,-88.9153259807367));
#17116=CARTESIAN_POINT('Ctrl Pts',(-47.9297652567514,152.652341336682,-89.0204439275952));
#17117=CARTESIAN_POINT('Ctrl Pts',(-47.4575992189624,152.800592378551,-89.2019737110398));
#17118=CARTESIAN_POINT('Ctrl Pts',(-46.9826690249351,152.947305215845,-89.3790749428026));
#17119=CARTESIAN_POINT('Ctrl Pts',(-46.5048664571461,153.092447219982,-89.5518784063299));
#17120=CARTESIAN_POINT('Ctrl Pts',(-46.0524027842201,153.22989203237,-89.715517731593));
#17121=CARTESIAN_POINT('Ctrl Pts',(-45.5969278339165,153.366049750584,-89.8754273982279));
#17122=CARTESIAN_POINT('Ctrl Pts',(-45.1392201295791,153.50064581587,-90.0314149120475));
#17123=CARTESIAN_POINT('Ctrl Pts',(-44.6903085940134,153.632655230997,-90.1844046775557));
#17124=CARTESIAN_POINT('Ctrl Pts',(-44.2394010756355,153.763116931994,-90.3335681685666));
#17125=CARTESIAN_POINT('Ctrl Pts',(-43.7875118830157,153.891695042633,-90.4786409992244));
#17126=CARTESIAN_POINT('Ctrl Pts',(-43.2921110680564,154.032653715327,-90.6376826397638));
#17127=CARTESIAN_POINT('Ctrl Pts',(-42.7955108465802,154.171367045258,-90.7918416708324));
#17128=CARTESIAN_POINT('Ctrl Pts',(-42.2979532665998,154.30775466438,-90.9411999794216));
#17129=CARTESIAN_POINT('Ctrl Pts',(-41.8806358039081,154.422147324535,-91.0664715718569));
#17130=CARTESIAN_POINT('Ctrl Pts',(-41.4625232501022,154.534937799496,-91.1884006026406));
#17131=CARTESIAN_POINT('Ctrl Pts',(-41.0436262570233,154.646114544382,-91.3070752601544));
#17132=CARTESIAN_POINT('Ctrl Pts',(-39.5524929062776,155.041866614378,-91.7295173942139));
#17133=CARTESIAN_POINT('Ctrl Pts',(-38.0514284305851,155.417169263234,-92.1107963665915));
#17134=CARTESIAN_POINT('Ctrl Pts',(-36.5408147180781,155.77152793962,-92.454022437313));
#17135=CARTESIAN_POINT('Ctrl Pts',(-36.1938322098199,155.852922846431,-92.5328602248509));
#17136=CARTESIAN_POINT('Ctrl Pts',(-35.8463458936313,155.93321278559,-92.6096870883139));
#17137=CARTESIAN_POINT('Ctrl Pts',(-35.4983599483625,156.01239194686,-92.684541040783));
#17138=CARTESIAN_POINT('Ctrl Pts',(-33.7317739216286,156.41435300825,-93.0645447400004));
#17139=CARTESIAN_POINT('Ctrl Pts',(-31.9523436552056,156.787699874605,-93.3939621738583));
#17140=CARTESIAN_POINT('Ctrl Pts',(-30.1603845094755,157.131655945597,-93.6757820461854));
#17141=CARTESIAN_POINT('Ctrl Pts',(-28.3684253637454,157.47561201659,-93.9576019185125));
#17142=CARTESIAN_POINT('Ctrl Pts',(-26.5639372568348,157.79017734767,-94.1918245741718));
#17143=CARTESIAN_POINT('Ctrl Pts',(-24.7472365628837,158.074585235959,-94.381496509228));
#17144=CARTESIAN_POINT('Ctrl Pts',(-24.5611024521864,158.103724878795,-94.4009297692435));
#17145=CARTESIAN_POINT('Ctrl Pts',(-24.3748401558089,158.132547950449,-94.4198947199084));
#17146=CARTESIAN_POINT('Ctrl Pts',(-24.1884499321931,158.161053644401,-94.4383946498845));
#17147=CARTESIAN_POINT('Ctrl Pts',(-21.8827037855024,158.51368423153,-94.6672486178073));
#17148=CARTESIAN_POINT('Ctrl Pts',(-19.5573481612408,158.817774755384,-94.8247861359747));
#17149=CARTESIAN_POINT('Ctrl Pts',(-17.2124345002704,159.071497582772,-94.9135091757608));
#17150=CARTESIAN_POINT('Ctrl Pts',(-15.6822612741615,159.237064393945,-94.9714053884356));
#17151=CARTESIAN_POINT('Ctrl Pts',(-14.1437598313738,159.381183387686,-95.));
#17152=CARTESIAN_POINT('Ctrl Pts',(-12.5969447708578,159.503344737469,-95.));
#17153=CARTESIAN_POINT('',(-12.5969447708577,159.503344737469,95.));
#17154=CARTESIAN_POINT('Ctrl Pts',(-12.5969447708577,159.503344737469,95.));
#17155=CARTESIAN_POINT('Ctrl Pts',(-14.9636417884215,159.316432345954,95.));
#17156=CARTESIAN_POINT('Ctrl Pts',(-17.3102321971143,159.0781682305,94.9330539868556));
#17157=CARTESIAN_POINT('Ctrl Pts',(-19.6366874222696,158.790458660472,94.7967566416616));
#17158=CARTESIAN_POINT('Ctrl Pts',(-21.1618309392931,158.601846225223,94.7074048199878));
#17159=CARTESIAN_POINT('Ctrl Pts',(-22.6783210761119,158.391983596727,94.5882491690846));
#17160=CARTESIAN_POINT('Ctrl Pts',(-24.1861500481769,158.161405361344,94.4386239423497));
#17161=CARTESIAN_POINT('Ctrl Pts',(-24.3718651728656,158.133005677741,94.4201950169514));
#17162=CARTESIAN_POINT('Ctrl Pts',(-24.5574491231664,158.104291546955,94.4013048160663));
#17163=CARTESIAN_POINT('Ctrl Pts',(-24.742901648231,158.075263811836,94.3819501633167));
#17164=CARTESIAN_POINT('Ctrl Pts',(-26.5589242771186,157.791013037557,94.1924219411736));
#17165=CARTESIAN_POINT('Ctrl Pts',(-28.3623429571352,157.476689937671,93.9584167982046));
#17166=CARTESIAN_POINT('Ctrl Pts',(-30.152843339076,157.13310297412,93.6769646228227));
#17167=CARTESIAN_POINT('Ctrl Pts',(-31.9433437210169,156.78951601057,93.3955124474409));
#17168=CARTESIAN_POINT('Ctrl Pts',(-33.7209258842786,156.416665133799,93.0666128972902));
#17169=CARTESIAN_POINT('Ctrl Pts',(-35.4852769954844,156.015368206333,92.6873548341285));
#17170=CARTESIAN_POINT('Ctrl Pts',(-35.8310461983781,155.936723928643,92.6130296290389));
#17171=CARTESIAN_POINT('Ctrl Pts',(-36.1763059771042,155.856986669202,92.5367605125138));
#17172=CARTESIAN_POINT('Ctrl Pts',(-36.5210521960025,155.776162483908,92.4585109007515));
#17173=CARTESIAN_POINT('Ctrl Pts',(-38.0313492281534,155.422080204005,92.1157075575005));
#17174=CARTESIAN_POINT('Ctrl Pts',(-39.531789681437,155.04713651561,91.7349542431376));
#17175=CARTESIAN_POINT('Ctrl Pts',(-41.0219877582951,154.651855858113,91.313202808891));
#17176=CARTESIAN_POINT('Ctrl Pts',(-41.437589578251,154.541615908673,91.1955804160267));
#17177=CARTESIAN_POINT('Ctrl Pts',(-41.8523940604112,154.429794280005,91.074763575325));
#17178=CARTESIAN_POINT('Ctrl Pts',(-42.2663906571552,154.316402951417,90.9506677174281));
#17179=CARTESIAN_POINT('Ctrl Pts',(-42.7657626262669,154.179627790745,90.8009805137071));
#17180=CARTESIAN_POINT('Ctrl Pts',(-43.263888543544,154.040588238986,90.6465480667306));
#17181=CARTESIAN_POINT('Ctrl Pts',(-43.7607921601594,153.899295220983,90.4872139652418));
#17182=CARTESIAN_POINT('Ctrl Pts',(-44.2084160951198,153.772014729181,90.3436815877405));
#17183=CARTESIAN_POINT('Ctrl Pts',(-44.6554133136073,153.642793503939,90.1960376830759));
#17184=CARTESIAN_POINT('Ctrl Pts',(-45.1011708062992,153.51183157811,90.0443759449032));
#17185=CARTESIAN_POINT('Ctrl Pts',(-45.5617485068334,153.376515529262,89.8876718720119));
#17186=CARTESIAN_POINT('Ctrl Pts',(-46.0211788417636,153.23928812832,89.7266157921222));
#17187=CARTESIAN_POINT('Ctrl Pts',(-46.4784104196994,153.100481269192,89.5614409688638));
#17188=CARTESIAN_POINT('Ctrl Pts',(-46.9549345962594,152.955817542015,89.3892966979082));
#17189=CARTESIAN_POINT('Ctrl Pts',(-47.4286966966318,152.809560712439,89.2128429647634));
#17190=CARTESIAN_POINT('Ctrl Pts',(-47.8993019180429,152.661902914232,89.0321483088218));
#17191=CARTESIAN_POINT('Ctrl Pts',(-48.9370157977482,152.33630825511,88.6337053168444));
#17192=CARTESIAN_POINT('Ctrl Pts',(-49.9607219667338,152.003487175208,88.2141700656783));
#17193=CARTESIAN_POINT('Ctrl Pts',(-50.9702419222352,151.664215661609,87.7727550423618));
#17194=CARTESIAN_POINT('Ctrl Pts',(-51.2399157194243,151.573585816353,87.6548395273436));
#17195=CARTESIAN_POINT('Ctrl Pts',(-51.5085772869238,151.48249561964,87.5353629667694));
#17196=CARTESIAN_POINT('Ctrl Pts',(-51.7762234015762,151.39095973765,87.4143109434925));
#17197=CARTESIAN_POINT('Ctrl Pts',(-52.7040666243346,151.07363419809,86.9946624104116));
#17198=CARTESIAN_POINT('Ctrl Pts',(-53.6197103208516,150.750948057866,86.5560940609331));
#17199=CARTESIAN_POINT('Ctrl Pts',(-54.522898061456,150.423576793448,86.0976450826551));
#17200=CARTESIAN_POINT('Ctrl Pts',(-55.3114117171572,150.137770530949,85.6974035120902));
#17201=CARTESIAN_POINT('Ctrl Pts',(-56.0904317952114,149.848393194912,85.2820098082707));
#17202=CARTESIAN_POINT('Ctrl Pts',(-56.8597968038474,149.55588757199,84.8508551158301));
#17203=CARTESIAN_POINT('Ctrl Pts',(-57.3859544162636,149.355847203052,84.5559946516678));
#17204=CARTESIAN_POINT('Ctrl Pts',(-57.9075999728538,149.154340665475,84.2537745826551));
#17205=CARTESIAN_POINT('Ctrl Pts',(-58.4246450085192,148.951533444028,83.9438875982944));
#17206=CARTESIAN_POINT('Ctrl Pts',(-59.1798215757925,148.65532083053,83.4912783032626));
#17207=CARTESIAN_POINT('Ctrl Pts',(-59.9251856576475,148.3563328907,83.0223558694528));
#17208=CARTESIAN_POINT('Ctrl Pts',(-60.6604276238275,148.055096320812,82.536209125394));
#17209=CARTESIAN_POINT('Ctrl Pts',(-61.0150211334615,147.909815532364,82.3017496030839));
#17210=CARTESIAN_POINT('Ctrl Pts',(-61.3672604880628,147.764011622712,82.0632845126909));
#17211=CARTESIAN_POINT('Ctrl Pts',(-61.7171120951143,147.617743088862,81.8207158106705));
#17212=CARTESIAN_POINT('Ctrl Pts',(-62.2383495586455,147.399820295193,81.4593171707193));
#17213=CARTESIAN_POINT('Ctrl Pts',(-62.7542769913379,147.180872854704,81.088778898013));
#17214=CARTESIAN_POINT('Ctrl Pts',(-63.2647378765564,146.961126802859,80.708636791763));
#17215=CARTESIAN_POINT('Ctrl Pts',(-63.5296293498669,146.847094842502,80.5113711333987));
#17216=CARTESIAN_POINT('Ctrl Pts',(-63.7931631002249,146.732798349721,80.3114362119227));
#17217=CARTESIAN_POINT('Ctrl Pts',(-64.0552014820334,146.618317965717,80.108854249111));
#17218=CARTESIAN_POINT('Ctrl Pts',(-64.4278584607107,146.455510083427,79.8207530111361));
#17219=CARTESIAN_POINT('Ctrl Pts',(-64.797203825589,146.292446583308,79.5274726487448));
#17220=CARTESIAN_POINT('Ctrl Pts',(-65.1621722401331,146.129699532309,79.2297442284713));
#17221=CARTESIAN_POINT('Ctrl Pts',(-65.297942280548,146.069156831048,79.1189877957436));
#17222=CARTESIAN_POINT('Ctrl Pts',(-65.4331070021292,146.008657850992,79.0076161106079));
#17223=CARTESIAN_POINT('Ctrl Pts',(-65.5676131150429,145.948231707859,78.8956678072283));
#17224=CARTESIAN_POINT('Ctrl Pts',(-65.8202507336994,145.834735625229,78.6853996479172));
#17225=CARTESIAN_POINT('Ctrl Pts',(-66.0707786683664,145.7214004756,78.4729134763841));
#17226=CARTESIAN_POINT('Ctrl Pts',(-66.3189251278449,145.608379463163,78.2583853065394));
#17227=CARTESIAN_POINT('Ctrl Pts',(-66.8077600897421,145.385734246204,77.8357765377006));
#17228=CARTESIAN_POINT('Ctrl Pts',(-67.2881427185282,145.163960479824,77.4047019300111));
#17229=CARTESIAN_POINT('Ctrl Pts',(-67.7597446135163,144.943488495273,76.965032086193));
#17230=CARTESIAN_POINT('Ctrl Pts',(-68.318258240347,144.682385626488,76.4443352830447));
#17231=CARTESIAN_POINT('Ctrl Pts',(-68.8645488295706,144.423066620625,75.9115540124255));
#17232=CARTESIAN_POINT('Ctrl Pts',(-69.3983709814738,144.166099904753,75.3662201410075));
#17233=CARTESIAN_POINT('Ctrl Pts',(-69.7852507803295,143.979867034883,74.9709973917619));
#17234=CARTESIAN_POINT('Ctrl Pts',(-70.1655820585078,143.794869292409,74.5691823587563));
#17235=CARTESIAN_POINT('Ctrl Pts',(-70.5392781657233,143.611316531388,74.1606111912411));
#17236=CARTESIAN_POINT('Ctrl Pts',(-70.9627708629114,143.403304587084,73.6975961841716));
#17237=CARTESIAN_POINT('Ctrl Pts',(-71.3777208982096,143.197162011134,73.2258699409069));
#17238=CARTESIAN_POINT('Ctrl Pts',(-71.7839076638945,142.993252942107,72.7450454092227));
#17239=CARTESIAN_POINT('Ctrl Pts',(-72.0208475537841,142.874307185022,72.4645672616853));
#17240=CARTESIAN_POINT('Ctrl Pts',(-72.2548059546961,142.756121130267,72.1809957430739));
#17241=CARTESIAN_POINT('Ctrl Pts',(-72.4857415364824,142.638764976099,71.8942661065626));
#17242=CARTESIAN_POINT('Ctrl Pts',(-72.8684374953895,142.444287686781,71.4191107738804));
#17243=CARTESIAN_POINT('Ctrl Pts',(-73.2428344044161,142.252088162916,70.9352862747557));
#17244=CARTESIAN_POINT('Ctrl Pts',(-73.6086679634405,142.062534534116,70.442372262658));
#17245=CARTESIAN_POINT('Ctrl Pts',(-73.8475013996346,141.938784967154,70.120574701025));
#17246=CARTESIAN_POINT('Ctrl Pts',(-74.0826769561078,141.816167236602,69.7949086505828));
#17247=CARTESIAN_POINT('Ctrl Pts',(-74.3141448724259,141.694770093608,69.4652303025532));
#17248=CARTESIAN_POINT('Ctrl Pts',(-74.5942217967198,141.547879159568,69.0663184395563));
#17249=CARTESIAN_POINT('Ctrl Pts',(-74.8691354183963,141.402625845848,68.6609941558653));
#17250=CARTESIAN_POINT('Ctrl Pts',(-75.1377859549508,141.259726775824,68.2506414100496));
#17251=CARTESIAN_POINT('Ctrl Pts',(-75.192420693496,141.230665775503,68.167189073544));
#17252=CARTESIAN_POINT('Ctrl Pts',(-75.2467964971052,141.201702079564,68.0835286394876));
#17253=CARTESIAN_POINT('Ctrl Pts',(-75.3009042600589,141.172841619946,67.9996715524561));
#17254=CARTESIAN_POINT('Ctrl Pts',(-75.5427668568644,141.043834887322,67.6248289841662));
#17255=CARTESIAN_POINT('Ctrl Pts',(-75.779235163084,140.916911689629,67.2461175539412));
#17256=CARTESIAN_POINT('Ctrl Pts',(-76.0095109018959,140.792593031219,66.8645514389451));
#17257=CARTESIAN_POINT('Ctrl Pts',(-76.4678093900085,140.545172032866,66.1051524049005));
#17258=CARTESIAN_POINT('Ctrl Pts',(-76.9030196715659,140.307330530175,65.3326162202851));
#17259=CARTESIAN_POINT('Ctrl Pts',(-77.314881639329,140.08000967159,64.5462581634978));
#17260=CARTESIAN_POINT('Ctrl Pts',(-77.3886533101512,140.039292536086,64.4054077032605));
#17261=CARTESIAN_POINT('Ctrl Pts',(-77.4616759218475,139.998912815778,64.2641138523276));
#17262=CARTESIAN_POINT('Ctrl Pts',(-77.5339480123353,139.958875765781,64.1223727486894));
#17263=CARTESIAN_POINT('Ctrl Pts',(-77.7608228970841,139.833192378979,63.6774223351203));
#17264=CARTESIAN_POINT('Ctrl Pts',(-77.9803042689531,139.710884654149,63.2280664572187));
#17265=CARTESIAN_POINT('Ctrl Pts',(-78.1922823959708,139.59214554871,62.774134193961));
#17266=CARTESIAN_POINT('Ctrl Pts',(-78.4291964078238,139.459438659422,62.2668039561155));
#17267=CARTESIAN_POINT('Ctrl Pts',(-78.656697695979,139.331212005233,61.7538460015109));
#17268=CARTESIAN_POINT('Ctrl Pts',(-78.8746118757149,139.207742605995,61.2351126948805));
#17269=CARTESIAN_POINT('Ctrl Pts',(-79.0457403477842,139.110781822329,60.8277503181747));
#17270=CARTESIAN_POINT('Ctrl Pts',(-79.2109597627441,139.016752899008,60.4168290717586));
#17271=CARTESIAN_POINT('Ctrl Pts',(-79.3701338567528,138.925814804349,60.0022364653027));
#17272=CARTESIAN_POINT('Ctrl Pts',(-79.5991272637939,138.794988087506,59.4057890717889));
#17273=CARTESIAN_POINT('Ctrl Pts',(-79.8155327390985,138.670602562738,58.8020121168909));
#17274=CARTESIAN_POINT('Ctrl Pts',(-80.0191366199309,138.553014310775,58.190105889466));
#17275=CARTESIAN_POINT('Ctrl Pts',(-80.1372766997562,138.484784346707,57.8350505228489));
#17276=CARTESIAN_POINT('Ctrl Pts',(-80.2512731188794,138.418744840624,57.4765876280007));
#17277=CARTESIAN_POINT('Ctrl Pts',(-80.3604379578907,138.35533929411,57.1167492175768));
#17278=CARTESIAN_POINT('Ctrl Pts',(-80.4119882901731,138.32539762955,56.9468246356937));
#17279=CARTESIAN_POINT('Ctrl Pts',(-80.4624757632866,138.296034849532,56.7765504471469));
#17280=CARTESIAN_POINT('Ctrl Pts',(-80.511824808259,138.267299337361,56.6061448214883));
#17281=CARTESIAN_POINT('Ctrl Pts',(-80.6661773762022,138.177421202995,56.0731548532513));
#17282=CARTESIAN_POINT('Ctrl Pts',(-80.80971869551,138.093493918004,55.5380894985181));
#17283=CARTESIAN_POINT('Ctrl Pts',(-80.9425086535139,138.015616119626,55.0009089778416));
#17284=CARTESIAN_POINT('Ctrl Pts',(-81.1848985336488,137.873460865587,54.0203595148038));
#17285=CARTESIAN_POINT('Ctrl Pts',(-81.3915079530963,137.751452856674,53.0327717650492));
#17286=CARTESIAN_POINT('Ctrl Pts',(-81.5622416952236,137.650284652651,52.0378044775898));
#17287=CARTESIAN_POINT('Ctrl Pts',(-81.5793285406492,137.640159849888,51.938229244056));
#17288=CARTESIAN_POINT('Ctrl Pts',(-81.5960560210763,137.630243783611,51.8385800942014));
#17289=CARTESIAN_POINT('Ctrl Pts',(-81.6124240130328,137.620537154591,51.7388566829908));
#17290=CARTESIAN_POINT('Ctrl Pts',(-81.6446771940527,137.601410210753,51.5423513790862));
#17291=CARTESIAN_POINT('Ctrl Pts',(-81.675534801156,137.583096367716,51.3455577967773));
#17292=CARTESIAN_POINT('Ctrl Pts',(-81.7049911434168,137.565602089959,51.1484722131202));
#17293=CARTESIAN_POINT('Ctrl Pts',(-81.840697101167,137.485005602549,50.240494988651));
#17294=CARTESIAN_POINT('Ctrl Pts',(-81.9466550214586,137.421808667808,49.3264666205647));
#17295=CARTESIAN_POINT('Ctrl Pts',(-82.0223229969576,137.376630218478,48.4062608221921));
#17296=CARTESIAN_POINT('Ctrl Pts',(-82.0939119350414,137.333887206121,47.5356606047341));
#17297=CARTESIAN_POINT('Ctrl Pts',(-82.1383964061816,137.307269356527,46.6595281125084));
#17298=CARTESIAN_POINT('Ctrl Pts',(-82.1548918638585,137.297394431107,45.777672594722));
#17299=CARTESIAN_POINT('Ctrl Pts',(-82.1597315135144,137.294497198405,45.5189424741761));
#17300=CARTESIAN_POINT('Ctrl Pts',(-82.1621621621139,137.293041006624,45.2597198077607));
#17301=CARTESIAN_POINT('Ctrl Pts',(-82.1621621621622,137.293041006595,45.0000000000001));
#17302=CARTESIAN_POINT('',(56.5922444183315,149.657334840949,95.));
#17303=CARTESIAN_POINT('Origin',(0.,0.,95.));
#17304=CARTESIAN_POINT('',(160.,3.36777869765522E-14,45.));
#17305=CARTESIAN_POINT('Ctrl Pts',(160.,3.36777869765522E-14,45.));
#17306=CARTESIAN_POINT('Ctrl Pts',(160.,0.244053147828224,45.0908288013671));
#17307=CARTESIAN_POINT('Ctrl Pts',(159.999433557959,0.492071829028524,45.1831334511064));
#17308=CARTESIAN_POINT('Ctrl Pts',(159.997155062312,0.985517893876185,45.3667780815545));
#17309=CARTESIAN_POINT('Ctrl Pts',(159.992026352869,1.72544209140982,45.6421534820189));
#17310=CARTESIAN_POINT('Ctrl Pts',(159.968105193101,3.45022173859571,46.2840540034421));
#17311=CARTESIAN_POINT('Ctrl Pts',(159.927183294251,4.92568645342637,46.8331493084511));
#17312=CARTESIAN_POINT('Ctrl Pts',(159.818287593492,7.87275838356731,47.9298532164966));
#17313=CARTESIAN_POINT('Ctrl Pts',(159.709630855535,9.83233101229018,48.6590074878283));
#17314=CARTESIAN_POINT('Ctrl Pts',(159.2765030292,15.6958359884224,50.8403997271284));
#17315=CARTESIAN_POINT('Ctrl Pts',(158.84502097174,19.5845746730536,52.2865796610741));
#17316=CARTESIAN_POINT('Ctrl Pts',(157.125137305964,31.190964030139,56.5994780417861));
#17317=CARTESIAN_POINT('Ctrl Pts',(155.413800322954,38.8490721013328,59.4408884221265));
#17318=CARTESIAN_POINT('Ctrl Pts',(152.828962450137,47.3739160272581,62.5917257526285));
#17319=CARTESIAN_POINT('Ctrl Pts',(152.532544816976,48.319857616323,62.9411763755992));
#17320=CARTESIAN_POINT('Ctrl Pts',(151.921104853419,50.2092000386463,63.638752880553));
#17321=CARTESIAN_POINT('Ctrl Pts',(151.60584962841,51.1532380133295,63.9871134500385));
#17322=CARTESIAN_POINT('Ctrl Pts',(150.63528262613,53.9718559190622,65.0265817145455));
#17323=CARTESIAN_POINT('Ctrl Pts',(149.954384630373,55.8355619005357,65.7130462914177));
#17324=CARTESIAN_POINT('Ctrl Pts',(147.810941106456,61.3810675999849,67.7526737154489));
#17325=CARTESIAN_POINT('Ctrl Pts',(146.24779276441,65.017314935261,69.0861171414286));
#17326=CARTESIAN_POINT('Ctrl Pts',(141.156919864418,75.7456037919146,73.004146909579));
#17327=CARTESIAN_POINT('Ctrl Pts',(137.230403745259,82.6581846336838,75.5075044348197));
#17328=CARTESIAN_POINT('Ctrl Pts',(131.623294985597,90.9908960669881,78.4763325219442));
#17329=CARTESIAN_POINT('Ctrl Pts',(130.466716096879,92.6419588132132,79.0619951565626));
#17330=CARTESIAN_POINT('Ctrl Pts',(128.677812363236,95.0949248954701,79.9275841406832));
#17331=CARTESIAN_POINT('Ctrl Pts',(128.071892999492,95.9094334951753,80.2142390390038));
#17332=CARTESIAN_POINT('Ctrl Pts',(126.845393169409,97.5257680899608,80.7814450557067));
#17333=CARTESIAN_POINT('Ctrl Pts',(126.224849980105,98.3275862731005,81.0619954633975));
#17334=CARTESIAN_POINT('Ctrl Pts',(123.085753077898,102.305078006677,82.4493004112037));
#17335=CARTESIAN_POINT('Ctrl Pts',(120.458236945284,105.386091967576,83.509847591627));
#17336=CARTESIAN_POINT('Ctrl Pts',(114.970035141697,111.347681824462,85.5255777952907));
#17337=CARTESIAN_POINT('Ctrl Pts',(112.109364020888,114.228261087591,86.4807952902017));
#17338=CARTESIAN_POINT('Ctrl Pts',(106.149377389369,119.786955934744,88.2752107002331));
#17339=CARTESIAN_POINT('Ctrl Pts',(103.05009718665,122.465087346466,89.1144688969865));
#17340=CARTESIAN_POINT('Ctrl Pts',(98.2139591883386,126.326059298113,90.2743768979733));
#17341=CARTESIAN_POINT('Ctrl Pts',(96.5704928774742,127.587107215203,90.6445055035526));
#17342=CARTESIAN_POINT('Ctrl Pts',(93.2197383402911,130.055412828185,91.3488393325667));
#17343=CARTESIAN_POINT('Ctrl Pts',(91.523272065474,131.254702876371,91.6807677118488));
#17344=CARTESIAN_POINT('Ctrl Pts',(86.3708892591745,134.749007104026,92.6132249860203));
#17345=CARTESIAN_POINT('Ctrl Pts',(82.8521059313916,136.940617783261,93.1507013044242));
#17346=CARTESIAN_POINT('Ctrl Pts',(75.6455579527511,141.049472945292,94.037579926942));
#17347=CARTESIAN_POINT('Ctrl Pts',(71.9578114879837,142.966725642616,94.3871133269088));
#17348=CARTESIAN_POINT('Ctrl Pts',(64.4081316590566,146.523048873891,94.8681992426883));
#17349=CARTESIAN_POINT('Ctrl Pts',(60.5462404390231,148.162149125729,95.));
#17350=CARTESIAN_POINT('Ctrl Pts',(56.5922444183315,149.657334840949,95.));
#17351=CARTESIAN_POINT('',(160.,-1.95943487863576E-14,125.));
#17352=CARTESIAN_POINT('',(160.,-1.95943487863576E-14,115.));
#17353=CARTESIAN_POINT('Origin',(0.,0.,125.));
#17354=CARTESIAN_POINT('',(160.,3.36777869765522E-14,-105.));
#17355=CARTESIAN_POINT('Origin',(-95.,158.745078663875,115.));
#17356=CARTESIAN_POINT('',(-80.,158.745078663875,-45.));
#17357=CARTESIAN_POINT('',(-93.125,173.627429788614,-45.));
#17358=CARTESIAN_POINT('Origin',(-95.,158.745078663875,-45.));
#17359=CARTESIAN_POINT('',(-87.2972972972973,145.873856069507,-45.));
#17360=CARTESIAN_POINT('Origin',(-95.,158.745078663875,-45.));
#17361=CARTESIAN_POINT('',(-87.2972972972973,145.873856069507,45.0000000000001));
#17362=CARTESIAN_POINT('',(-87.2972972972972,145.873856069507,115.));
#17363=CARTESIAN_POINT('',(-80.,158.745078663875,45.0000000000001));
#17364=CARTESIAN_POINT('Origin',(-95.,158.745078663875,45.0000000000001));
#17365=CARTESIAN_POINT('',(-93.125,173.627429788614,45.0000000000001));
#17366=CARTESIAN_POINT('Origin',(-95.,158.745078663875,45.0000000000001));
#17367=CARTESIAN_POINT('',(-93.125,173.627429788614,-105.));
#17368=CARTESIAN_POINT('Origin',(0.,0.,115.));
#17369=CARTESIAN_POINT('',(170.,0.,-45.));
#17370=CARTESIAN_POINT('',(170.,-2.0818995585505E-14,115.));
#17371=CARTESIAN_POINT('',(170.,0.,45.));
#17372=CARTESIAN_POINT('',(170.,0.,-80.));
#17373=CARTESIAN_POINT('',(170.,-2.0818995585505E-14,115.));
#17374=CARTESIAN_POINT('',(170.,-2.0818995585505E-14,115.));
#17375=CARTESIAN_POINT('Origin',(0.,0.,115.));
#17376=CARTESIAN_POINT('',(60.1292596944772,159.010918268508,95.));
#17377=CARTESIAN_POINT('Ctrl Pts',(170.,0.,45.));
#17378=CARTESIAN_POINT('Ctrl Pts',(170.,0.26003052026448,45.091082419179));
#17379=CARTESIAN_POINT('Ctrl Pts',(169.999394183212,0.524501631954243,45.1837202730264));
#17380=CARTESIAN_POINT('Ctrl Pts',(169.996958612046,1.05032722296935,45.3679040271418));
#17381=CARTESIAN_POINT('Ctrl Pts',(169.991476684799,1.83880024712644,45.6440863033289));
#17382=CARTESIAN_POINT('Ctrl Pts',(169.965910091794,3.67671754845105,46.2878568548837));
#17383=CARTESIAN_POINT('Ctrl Pts',(169.922176515592,5.24891333774521,46.8385332643445));
#17384=CARTESIAN_POINT('Ctrl Pts',(169.80580451179,8.38912428069815,47.9383702016001));
#17385=CARTESIAN_POINT('Ctrl Pts',(169.689693680506,10.47702552627,48.6695742664345));
#17386=CARTESIAN_POINT('Ctrl Pts',(169.22689115823,16.7242377993534,50.85699761865));
#17387=CARTESIAN_POINT('Ctrl Pts',(168.765886558002,20.8670784878288,52.3070408841403));
#17388=CARTESIAN_POINT('Ctrl Pts',(166.928601437382,33.2307048294446,56.6310354999103));
#17389=CARTESIAN_POINT('Ctrl Pts',(165.100719651717,41.3869108937082,59.4791921961275));
#17390=CARTESIAN_POINT('Ctrl Pts',(162.340601127124,50.4642501038184,62.6367460390978));
#17391=CARTESIAN_POINT('Ctrl Pts',(162.024090898783,51.4714701492619,62.9869306646656));
#17392=CARTESIAN_POINT('Ctrl Pts',(161.371221757297,53.4831474341294,63.6859498503516));
#17393=CARTESIAN_POINT('Ctrl Pts',(161.034658418127,54.4881463629123,64.0349720718961));
#17394=CARTESIAN_POINT('Ctrl Pts',(159.99868842936,57.488232922231,65.0762222429013));
#17395=CARTESIAN_POINT('Ctrl Pts',(159.272002630726,59.4716702238614,65.7637685033219));
#17396=CARTESIAN_POINT('Ctrl Pts',(156.984757165518,65.3726819287223,67.8063284591325));
#17397=CARTESIAN_POINT('Ctrl Pts',(155.317165023605,69.2410214317241,69.1413108297163));
#17398=CARTESIAN_POINT('Ctrl Pts',(149.887841477183,80.6510891236089,73.0627350000645));
#17399=CARTESIAN_POINT('Ctrl Pts',(145.702324214992,87.9989448939223,75.5667325529025));
#17400=CARTESIAN_POINT('Ctrl Pts',(139.729767240726,96.8511925371005,78.5342884232701));
#17401=CARTESIAN_POINT('Ctrl Pts',(138.498003901055,98.604927815123,79.1195924508518));
#17402=CARTESIAN_POINT('Ctrl Pts',(136.593151713623,101.210019876689,79.9844850983316));
#17403=CARTESIAN_POINT('Ctrl Pts',(135.948034234115,102.074941840187,80.2708709224333));
#17404=CARTESIAN_POINT('Ctrl Pts',(134.642784559476,103.790569561344,80.837287641356));
#17405=CARTESIAN_POINT('Ctrl Pts',(133.982461046718,104.641574331305,81.117419484298));
#17406=CARTESIAN_POINT('Ctrl Pts',(130.642458316523,108.862717363317,82.5025158428281));
#17407=CARTESIAN_POINT('Ctrl Pts',(127.847811255468,112.131361115642,83.5609252410729));
#17408=CARTESIAN_POINT('Ctrl Pts',(122.012996265914,118.453930836736,85.5717401251865));
#17409=CARTESIAN_POINT('Ctrl Pts',(118.972841259923,121.507859522579,86.5241790265868));
#17410=CARTESIAN_POINT('Ctrl Pts',(112.641836965441,127.399032367865,88.3125256163411));
#17411=CARTESIAN_POINT('Ctrl Pts',(109.351021141409,130.236292245747,89.1484916842017));
#17412=CARTESIAN_POINT('Ctrl Pts',(104.218688827331,134.325162608347,90.3032259939414));
#17413=CARTESIAN_POINT('Ctrl Pts',(102.474476255975,135.660766282279,90.6716939178001));
#17414=CARTESIAN_POINT('Ctrl Pts',(98.921480159219,138.272927774531,91.3722444352154));
#17415=CARTESIAN_POINT('Ctrl Pts',(97.122876159534,139.542038720585,91.702332993713));
#17416=CARTESIAN_POINT('Ctrl Pts',(91.6611011033309,143.239579445468,92.6294671833747));
#17417=CARTESIAN_POINT('Ctrl Pts',(87.9320862659756,145.558387389969,93.1636516044368));
#17418=CARTESIAN_POINT('Ctrl Pts',(80.2974529965281,149.905353396487,94.044773738069));
#17419=CARTESIAN_POINT('Ctrl Pts',(76.3918510029905,151.933518732781,94.3918381893336));
#17420=CARTESIAN_POINT('Ctrl Pts',(68.3991059160043,155.695444133984,94.8693319054603));
#17421=CARTESIAN_POINT('Ctrl Pts',(64.3120020922313,157.429233145195,95.));
#17422=CARTESIAN_POINT('Ctrl Pts',(60.1292596944772,159.010918268508,95.));
#17423=CARTESIAN_POINT('',(-13.3842538190363,169.472303783561,95.));
#17424=CARTESIAN_POINT('Origin',(0.,0.,95.));
#17425=CARTESIAN_POINT('Ctrl Pts',(-13.3842538190363,169.472303783561,95.));
#17426=CARTESIAN_POINT('Ctrl Pts',(-16.3602967714103,169.237267654579,95.));
#17427=CARTESIAN_POINT('Ctrl Pts',(-19.3081742236088,168.925670678062,94.9062326532765));
#17428=CARTESIAN_POINT('Ctrl Pts',(-22.2278148953825,168.540593873598,94.7143704136405));
#17429=CARTESIAN_POINT('Ctrl Pts',(-23.3889397061482,168.387450976242,94.6380678710557));
#17430=CARTESIAN_POINT('Ctrl Pts',(-24.545598563398,168.222686262647,94.5462511008142));
#17431=CARTESIAN_POINT('Ctrl Pts',(-25.6977869660726,168.046492807987,94.4386500863327));
#17432=CARTESIAN_POINT('Ctrl Pts',(-25.8082073233279,168.029607249892,94.428338107465));
#17433=CARTESIAN_POINT('Ctrl Pts',(-25.9185866942024,168.012616663519,94.417881455326));
#17434=CARTESIAN_POINT('Ctrl Pts',(-26.0289250306962,167.995521189932,94.4072795523634));
#17435=CARTESIAN_POINT('Ctrl Pts',(-28.1898062203598,167.66072107896,94.1996504234983));
#17436=CARTESIAN_POINT('Ctrl Pts',(-30.3349411351003,167.28569316815,93.9363563245313));
#17437=CARTESIAN_POINT('Ctrl Pts',(-32.4638933110135,166.871514180024,93.6130702105055));
#17438=CARTESIAN_POINT('Ctrl Pts',(-34.221408510367,166.529596745184,93.3461876259324));
#17439=CARTESIAN_POINT('Ctrl Pts',(-35.9678952264575,166.160997957463,93.0384211810286));
#17440=CARTESIAN_POINT('Ctrl Pts',(-37.7031085064815,165.766328332842,92.6873629078737));
#17441=CARTESIAN_POINT('Ctrl Pts',(-37.9092616110374,165.719439359984,92.6456552090426));
#17442=CARTESIAN_POINT('Ctrl Pts',(-38.1152551687545,165.672182239619,92.6033333314582));
#17443=CARTESIAN_POINT('Ctrl Pts',(-38.3210884337155,165.624557972509,92.5603906152076));
#17444=CARTESIAN_POINT('Ctrl Pts',(-40.0879915027861,165.215744247801,92.1917640127398));
#17445=CARTESIAN_POINT('Ctrl Pts',(-41.8430834916924,164.779875427169,91.7774366479129));
#17446=CARTESIAN_POINT('Ctrl Pts',(-43.5858629304468,164.317596600633,91.3132064962846));
#17447=CARTESIAN_POINT('Ctrl Pts',(-43.8340397160827,164.251766771175,91.2470987925417));
#17448=CARTESIAN_POINT('Ctrl Pts',(-44.0819665865614,164.185401421503,91.179977322963));
#17449=CARTESIAN_POINT('Ctrl Pts',(-44.3296416785955,164.118502515818,91.1118266024519));
#17450=CARTESIAN_POINT('Ctrl Pts',(-45.0538775881994,163.922880948011,90.9125445565501));
#17451=CARTESIAN_POINT('Ctrl Pts',(-45.7760781643882,163.722663714208,90.7044316798228));
#17452=CARTESIAN_POINT('Ctrl Pts',(-46.4958413663918,163.518001258673,90.4872126994076));
#17453=CARTESIAN_POINT('Ctrl Pts',(-46.7634084940561,163.441919367829,90.4064630049218));
#17454=CARTESIAN_POINT('Ctrl Pts',(-47.0307617265755,163.365185663339,90.3244129008275));
#17455=CARTESIAN_POINT('Ctrl Pts',(-47.2977613961294,163.287845073462,90.2410869824901));
#17456=CARTESIAN_POINT('Ctrl Pts',(-47.8655785725555,163.12336803332,90.0638811913652));
#17457=CARTESIAN_POINT('Ctrl Pts',(-48.4324760349077,162.955947512629,89.8806886779588));
#17458=CARTESIAN_POINT('Ctrl Pts',(-48.9967296166451,162.786117367686,89.6918458325172));
#17459=CARTESIAN_POINT('Ctrl Pts',(-49.1257349206187,162.747289099366,89.6486706902267));
#17460=CARTESIAN_POINT('Ctrl Pts',(-49.2546020849577,162.708334961929,89.6052003831832));
#17461=CARTESIAN_POINT('Ctrl Pts',(-49.383310644726,162.669261477904,89.5614392605881));
#17462=CARTESIAN_POINT('Ctrl Pts',(-49.6684474558472,162.582699335851,89.4644922745422));
#17463=CARTESIAN_POINT('Ctrl Pts',(-49.9526798261573,162.495592644993,89.3661699692017));
#17464=CARTESIAN_POINT('Ctrl Pts',(-50.2359343342916,162.407976313914,89.2664815691616));
#17465=CARTESIAN_POINT('Ctrl Pts',(-51.5020145058062,162.016352186871,88.8208981697932));
#17466=CARTESIAN_POINT('Ctrl Pts',(-52.7500857914976,161.614076535672,88.3475284276466));
#17467=CARTESIAN_POINT('Ctrl Pts',(-53.9798246569649,161.202290116088,87.8449659507344));
#17468=CARTESIAN_POINT('Ctrl Pts',(-54.325413657281,161.086567289816,87.7037326622131));
#17469=CARTESIAN_POINT('Ctrl Pts',(-54.669554935815,160.970093287806,87.5601941484649));
#17470=CARTESIAN_POINT('Ctrl Pts',(-55.0122415374991,160.852893293963,87.4143198954764));
#17471=CARTESIAN_POINT('Ctrl Pts',(-56.13874522836,160.467625165638,86.934791709707));
#17472=CARTESIAN_POINT('Ctrl Pts',(-57.2495354683247,160.074505380291,86.4300424847287));
#17473=CARTESIAN_POINT('Ctrl Pts',(-58.3441670040107,159.67453463909,85.8984368616859));
#17474=CARTESIAN_POINT('Ctrl Pts',(-59.0405329442612,159.420087373331,85.5602481310819));
#17475=CARTESIAN_POINT('Ctrl Pts',(-59.7303596715798,159.162867298507,85.2111914083026));
#17476=CARTESIAN_POINT('Ctrl Pts',(-60.4135358107492,158.903129896419,84.8508559644503));
#17477=CARTESIAN_POINT('Ctrl Pts',(-60.7310756209656,158.782404126538,84.6833722923855));
#17478=CARTESIAN_POINT('Ctrl Pts',(-61.0471798789429,158.661133474286,84.5134557611085));
#17479=CARTESIAN_POINT('Ctrl Pts',(-61.3618299268532,158.539348482521,84.3410435386296));
#17480=CARTESIAN_POINT('Ctrl Pts',(-62.2894869232013,158.180299753905,83.8327346872544));
#17481=CARTESIAN_POINT('Ctrl Pts',(-63.2045107694617,157.816777747238,83.3027807982613));
#17482=CARTESIAN_POINT('Ctrl Pts',(-64.1063866299605,157.449578057315,82.7495954719335));
#17483=CARTESIAN_POINT('Ctrl Pts',(-64.5997003097787,157.248724882063,82.4470107139811));
#17484=CARTESIAN_POINT('Ctrl Pts',(-65.0890804065802,157.046771276094,82.1374760952267));
#17485=CARTESIAN_POINT('Ctrl Pts',(-65.5744442404841,156.843846747502,81.820738416781));
#17486=CARTESIAN_POINT('Ctrl Pts',(-65.890670864759,156.711636363915,81.6143759319004));
#17487=CARTESIAN_POINT('Ctrl Pts',(-66.2051893463786,156.579016099359,81.4049462447273));
#17488=CARTESIAN_POINT('Ctrl Pts',(-66.5179674014292,156.446028480324,81.1923519764314));
#17489=CARTESIAN_POINT('Ctrl Pts',(-67.0362519774947,156.22566317451,80.8400755668865));
#17490=CARTESIAN_POINT('Ctrl Pts',(-67.5499166828611,156.004220985238,80.4790186029946));
#17491=CARTESIAN_POINT('Ctrl Pts',(-68.0586509128982,155.781963127688,80.1088529719505));
#17492=CARTESIAN_POINT('Ctrl Pts',(-68.3697825255568,155.646034696766,79.8824671246112));
#17493=CARTESIAN_POINT('Ctrl Pts',(-68.678883121499,155.50987721189,79.6527834047028));
#17494=CARTESIAN_POINT('Ctrl Pts',(-68.9855269800791,155.373726306775,79.4200399155403));
#17495=CARTESIAN_POINT('Ctrl Pts',(-69.4459231453065,155.169308860109,79.0705980242588));
#17496=CARTESIAN_POINT('Ctrl Pts',(-69.9004164530957,154.965069720224,78.7145458423159));
#17497=CARTESIAN_POINT('Ctrl Pts',(-70.3480524083544,154.761595478826,78.3523496618931));
#17498=CARTESIAN_POINT('Ctrl Pts',(-70.3867057728156,154.744025478206,78.3210740219363));
#17499=CARTESIAN_POINT('Ctrl Pts',(-70.4253080005176,154.726461174113,78.2897525398122));
#17500=CARTESIAN_POINT('Ctrl Pts',(-70.463858472605,154.708902940828,78.2583854988648));
#17501=CARTESIAN_POINT('Ctrl Pts',(-70.762416999286,154.572921201129,78.0154598737167));
#17502=CARTESIAN_POINT('Ctrl Pts',(-71.0581493646474,154.437181403389,77.7696245694438));
#17503=CARTESIAN_POINT('Ctrl Pts',(-71.3511110895723,154.301710155538,77.5207217504554));
#17504=CARTESIAN_POINT('Ctrl Pts',(-72.0300168261834,153.987770826653,76.9439175562788));
#17505=CARTESIAN_POINT('Ctrl Pts',(-72.6935068910743,153.675521193897,76.351201597096));
#17506=CARTESIAN_POINT('Ctrl Pts',(-73.3411064736323,153.365835369114,75.741687555929));
#17507=CARTESIAN_POINT('Ctrl Pts',(-73.8881569515263,153.104232701343,75.2268092939844));
#17508=CARTESIAN_POINT('Ctrl Pts',(-74.4238686181605,152.844459258757,74.699944915077));
#17509=CARTESIAN_POINT('Ctrl Pts',(-74.9479655229901,152.587032424301,74.1605856133349));
#17510=CARTESIAN_POINT('Ctrl Pts',(-75.2087163460111,152.458956378948,73.8922413805464));
#17511=CARTESIAN_POINT('Ctrl Pts',(-75.4665990358862,152.33145637757,73.6208150897529));
#17512=CARTESIAN_POINT('Ctrl Pts',(-75.7215484874426,152.204616299458,73.3461973876455));
#17513=CARTESIAN_POINT('Ctrl Pts',(-76.322479956938,151.905646468125,72.6989066471895));
#17514=CARTESIAN_POINT('Ctrl Pts',(-76.9070841752639,151.610359645666,72.0340893553267));
#17515=CARTESIAN_POINT('Ctrl Pts',(-77.4746362476924,151.319781418506,71.3502680491987));
#17516=CARTESIAN_POINT('Ctrl Pts',(-77.9832035397331,151.05940252238,70.7375151992105));
#17517=CARTESIAN_POINT('Ctrl Pts',(-78.4780791420081,150.802803992481,70.1095037375267));
#17518=CARTESIAN_POINT('Ctrl Pts',(-78.9587508849806,150.550707931619,69.4652010508605));
#17519=CARTESIAN_POINT('Ctrl Pts',(-79.168166589072,150.440876482494,69.1844957613384));
#17520=CARTESIAN_POINT('Ctrl Pts',(-79.3750144085231,150.331828466866,68.9004120357299));
#17521=CARTESIAN_POINT('Ctrl Pts',(-79.5788665952709,150.223838104592,68.6134266440515));
#17522=CARTESIAN_POINT('Ctrl Pts',(-79.9006718636303,150.053362290393,68.1603855829883));
#17523=CARTESIAN_POINT('Ctrl Pts',(-80.2149120831088,149.885575415521,67.7002696808478));
#17524=CARTESIAN_POINT('Ctrl Pts',(-80.5200023905008,149.721503208657,67.2348659577922));
#17525=CARTESIAN_POINT('Ctrl Pts',(-80.6006857382064,149.678113121872,67.1117865629343));
#17526=CARTESIAN_POINT('Ctrl Pts',(-80.6807292784571,149.634982740388,66.9883371043634));
#17527=CARTESIAN_POINT('Ctrl Pts',(-80.7601039316535,149.592130852357,66.8645501211407));
#17528=CARTESIAN_POINT('Ctrl Pts',(-80.9373628184296,149.496434333849,66.5881099483674));
#17529=CARTESIAN_POINT('Ctrl Pts',(-81.1114879618528,149.402022980671,66.3097454001126));
#17530=CARTESIAN_POINT('Ctrl Pts',(-81.2824610346225,149.308946880817,66.0294022553307));
#17531=CARTESIAN_POINT('Ctrl Pts',(-81.6641120200211,149.101179747369,65.4036122655823));
#17532=CARTESIAN_POINT('Ctrl Pts',(-82.0300183432883,148.900087324285,64.7680540995119));
#17533=CARTESIAN_POINT('Ctrl Pts',(-82.3798221155295,148.706304197954,64.1223741806755));
#17534=CARTESIAN_POINT('Ctrl Pts',(-82.5222365974763,148.627409898532,63.8595005971364));
#17535=CARTESIAN_POINT('Ctrl Pts',(-82.6619832251089,148.549726352339,63.5949503331329));
#17536=CARTESIAN_POINT('Ctrl Pts',(-82.7990243480897,148.473302833396,63.3286896484053));
#17537=CARTESIAN_POINT('Ctrl Pts',(-83.1522801825168,148.276303178352,62.6423398994197));
#17538=CARTESIAN_POINT('Ctrl Pts',(-83.4875625884937,148.087674689848,61.9446586895439));
#17539=CARTESIAN_POINT('Ctrl Pts',(-83.8042673895934,147.908230897748,61.2351072858843));
#17540=CARTESIAN_POINT('Ctrl Pts',(-84.0985651096953,147.741482876506,60.5757571286811));
#17541=CARTESIAN_POINT('Ctrl Pts',(-84.3768294699192,147.582661074393,59.9061636400998));
#17542=CARTESIAN_POINT('Ctrl Pts',(-84.6383399601401,147.432532301283,59.2257173412033));
#17543=CARTESIAN_POINT('Ctrl Pts',(-84.7699435606084,147.356980888188,58.8832867840793));
#17544=CARTESIAN_POINT('Ctrl Pts',(-84.8973046834799,147.283630599417,58.5381081607792));
#17545=CARTESIAN_POINT('Ctrl Pts',(-85.0203346904952,147.212576531754,58.1901066250535));
#17546=CARTESIAN_POINT('Ctrl Pts',(-85.0952405390784,147.169315823552,57.9782286371204));
#17547=CARTESIAN_POINT('Ctrl Pts',(-85.1686045115591,147.126868896399,57.7650647152473));
#17548=CARTESIAN_POINT('Ctrl Pts',(-85.2402620956793,147.085341132009,57.5510665884564));
#17549=CARTESIAN_POINT('Ctrl Pts',(-85.3452374681436,147.024504688973,57.2375682568791));
#17550=CARTESIAN_POINT('Ctrl Pts',(-85.4465991137606,146.96561284564,56.9221345842854));
#17551=CARTESIAN_POINT('Ctrl Pts',(-85.5438296400012,146.908996356665,56.6061514339965));
#17552=CARTESIAN_POINT('Ctrl Pts',(-85.7077466516527,146.813548907784,56.0734482210215));
#17553=CARTESIAN_POINT('Ctrl Pts',(-85.8602690201768,146.724370794082,55.5383934624432));
#17554=CARTESIAN_POINT('Ctrl Pts',(-86.0014326176293,146.641582055417,55.0009151052429));
#17555=CARTESIAN_POINT('Ctrl Pts',(-86.0457044679173,146.615617779146,54.8323506750891));
#17556=CARTESIAN_POINT('Ctrl Pts',(-86.088860270053,146.590281706134,54.6635481162933));
#17557=CARTESIAN_POINT('Ctrl Pts',(-86.1308986805349,146.5655780796,54.4945046808591));
#17558=CARTESIAN_POINT('Ctrl Pts',(-86.35758732035,146.432365823636,53.5829519839561));
#17559=CARTESIAN_POINT('Ctrl Pts',(-86.5517922493526,146.317539877232,52.6644417912851));
#17560=CARTESIAN_POINT('Ctrl Pts',(-86.7132062820898,146.221817306037,51.7388579964434));
#17561=CARTESIAN_POINT('Ctrl Pts',(-86.7337856955697,146.209613197519,51.6208510840248));
#17562=CARTESIAN_POINT('Ctrl Pts',(-86.7538322187789,146.197719546278,51.5027292367629));
#17563=CARTESIAN_POINT('Ctrl Pts',(-86.7733441493221,146.186138071075,51.3844919987536));
#17564=CARTESIAN_POINT('Ctrl Pts',(-86.9358369512435,146.089689062511,50.3998277671451));
#17565=CARTESIAN_POINT('Ctrl Pts',(-87.0612765053318,146.014877687189,49.4071627883501));
#17566=CARTESIAN_POINT('Ctrl Pts',(-87.1487224382178,145.962667067261,48.406261267487));
#17567=CARTESIAN_POINT('Ctrl Pts',(-87.2321973497412,145.912827392215,47.4508118470259));
#17568=CARTESIAN_POINT('Ctrl Pts',(-87.2810611497313,145.883578565544,46.4878534783608));
#17569=CARTESIAN_POINT('Ctrl Pts',(-87.293883511954,145.875900574328,45.5170658868486));
#17570=CARTESIAN_POINT('Ctrl Pts',(-87.2961567586591,145.874539361165,45.3449572179969));
#17571=CARTESIAN_POINT('Ctrl Pts',(-87.2972972972612,145.873856069529,45.1726025028241));
#17572=CARTESIAN_POINT('Ctrl Pts',(-87.2972972972973,145.873856069507,45.0000000000001));
#17573=CARTESIAN_POINT('',(-13.3842538190364,169.472303783561,-95.));
#17574=CARTESIAN_POINT('Ctrl Pts',(-87.2972972972973,145.873856069507,-45.));
#17575=CARTESIAN_POINT('Ctrl Pts',(-87.2972972972127,145.873856069558,-45.9848836362899));
#17576=CARTESIAN_POINT('Ctrl Pts',(-87.2601578418064,145.896106375359,-46.9618714459115));
#17577=CARTESIAN_POINT('Ctrl Pts',(-87.1873161145765,145.939618737676,-47.9312779503657));
#17578=CARTESIAN_POINT('Ctrl Pts',(-87.1753834170317,145.946746792964,-48.0900830069663));
#17579=CARTESIAN_POINT('Ctrl Pts',(-87.1624927075728,145.954445375665,-48.2486846405294));
#17580=CARTESIAN_POINT('Ctrl Pts',(-87.1486504118183,145.962710071443,-48.4070842669367));
#17581=CARTESIAN_POINT('Ctrl Pts',(-87.0614449138588,146.014777078506,-49.4049908672901));
#17582=CARTESIAN_POINT('Ctrl Pts',(-86.9364575008243,146.089318977909,-50.3948826080192));
#17583=CARTESIAN_POINT('Ctrl Pts',(-86.7745829867444,146.185402758173,-51.376980415473));
#17584=CARTESIAN_POINT('Ctrl Pts',(-86.7545092707146,146.197317904488,-51.4987682868518));
#17585=CARTESIAN_POINT('Ctrl Pts',(-86.7338679528499,146.209564522444,-51.6204362722608));
#17586=CARTESIAN_POINT('Ctrl Pts',(-86.7126608231955,146.222140775472,-51.7419848435814));
#17587=CARTESIAN_POINT('Ctrl Pts',(-86.55193500937,146.31745440517,-52.6631841460454));
#17588=CARTESIAN_POINT('Ctrl Pts',(-86.3587024471325,146.431705790483,-53.5775217053184));
#17589=CARTESIAN_POINT('Ctrl Pts',(-86.1332375713659,146.564203662116,-54.4851039931522));
#17590=CARTESIAN_POINT('Ctrl Pts',(-86.0899027947026,146.589670004295,-54.6595430298897));
#17591=CARTESIAN_POINT('Ctrl Pts',(-86.0453761108919,146.615811080381,-54.8337323062595));
#17592=CARTESIAN_POINT('Ctrl Pts',(-85.9996595589194,146.642621893329,-55.0076726367092));
#17593=CARTESIAN_POINT('Ctrl Pts',(-85.9107555125789,146.694760334527,-55.3459308502346));
#17594=CARTESIAN_POINT('Ctrl Pts',(-85.8173466193961,146.749432661039,-55.6832465331334));
#17595=CARTESIAN_POINT('Ctrl Pts',(-85.71942978857,146.806605547736,-56.0196221499469));
#17596=CARTESIAN_POINT('Ctrl Pts',(-85.6615625704552,146.840393772669,-56.2184145436795));
#17597=CARTESIAN_POINT('Ctrl Pts',(-85.602098822783,146.87506822937,-56.4169525834863));
#17598=CARTESIAN_POINT('Ctrl Pts',(-85.5410516857225,146.910613900087,-56.6151812431414));
#17599=CARTESIAN_POINT('Ctrl Pts',(-85.445683233865,146.966143704592,-56.9248560501086));
#17600=CARTESIAN_POINT('Ctrl Pts',(-85.3464897727364,147.023775596745,-57.2335577883328));
#17601=CARTESIAN_POINT('Ctrl Pts',(-85.2439494976614,147.083204214466,-57.5400724674477));
#17602=CARTESIAN_POINT('Ctrl Pts',(-85.1701205745959,147.125992775765,-57.7607628122539));
#17603=CARTESIAN_POINT('Ctrl Pts',(-85.0944922004626,147.169750155055,-57.9805153356884));
#17604=CARTESIAN_POINT('Ctrl Pts',(-85.0172143876343,147.214378570055,-58.1989426996576));
#17605=CARTESIAN_POINT('Ctrl Pts',(-84.7981706813637,147.340877665574,-58.8180743443513));
#17606=CARTESIAN_POINT('Ctrl Pts',(-84.5652672651916,147.474731098872,-59.4286784047483));
#17607=CARTESIAN_POINT('Ctrl Pts',(-84.3190010331543,147.615399903826,-60.0310545986629));
#17608=CARTESIAN_POINT('Ctrl Pts',(-84.1522200733756,147.710666226403,-60.4390069148932));
#17609=CARTESIAN_POINT('Ctrl Pts',(-83.9793110000177,147.809057875933,-60.8431861352841));
#17610=CARTESIAN_POINT('Ctrl Pts',(-83.8004373335544,147.9104009281,-61.2436928500744));
#17611=CARTESIAN_POINT('Ctrl Pts',(-83.5213153281546,148.068540896455,-61.8686604018594));
#17612=CARTESIAN_POINT('Ctrl Pts',(-83.227660732651,148.233872659777,-62.4846786679934));
#17613=CARTESIAN_POINT('Ctrl Pts',(-82.9199078493258,148.405825476924,-63.0919942464788));
#17614=CARTESIAN_POINT('Ctrl Pts',(-82.8826975341711,148.426616244011,-63.1654246034251));
#17615=CARTESIAN_POINT('Ctrl Pts',(-82.8452811563684,148.447503775454,-63.2387277690164));
#17616=CARTESIAN_POINT('Ctrl Pts',(-82.8076595183652,148.468487038094,-63.3119042074312));
#17617=CARTESIAN_POINT('Ctrl Pts',(-82.6657598925264,148.547630777586,-63.5879078527379));
#17618=CARTESIAN_POINT('Ctrl Pts',(-82.5209294596415,148.628142417463,-63.8621216215528));
#17619=CARTESIAN_POINT('Ctrl Pts',(-82.3732072730211,148.709968474063,-64.1345800057147));
#17620=CARTESIAN_POINT('Ctrl Pts',(-82.0282675642021,148.901036970834,-64.7707858313133));
#17621=CARTESIAN_POINT('Ctrl Pts',(-81.6675541821605,149.099276572551,-65.3974150592188));
#17622=CARTESIAN_POINT('Ctrl Pts',(-81.2913777116218,149.304092491018,-66.0147759266973));
#17623=CARTESIAN_POINT('Ctrl Pts',(-81.1136958590786,149.400834511515,-66.3063779571596));
#17624=CARTESIAN_POINT('Ctrl Pts',(-80.932568038796,149.499041513155,-66.5958998850957));
#17625=CARTESIAN_POINT('Ctrl Pts',(-80.7480156183748,149.59865632316,-66.8833928168321));
#17626=CARTESIAN_POINT('Ctrl Pts',(-80.4944836312975,149.735503841415,-67.2783410601955));
#17627=CARTESIAN_POINT('Ctrl Pts',(-80.2341755442533,149.875171570879,-67.6698536656852));
#17628=CARTESIAN_POINT('Ctrl Pts',(-79.9689674067322,150.016546384168,-68.0554758763857));
#17629=CARTESIAN_POINT('Ctrl Pts',(-79.9345638834303,150.034885910733,-68.1054998418476));
#17630=CARTESIAN_POINT('Ctrl Pts',(-79.9000779383347,150.053254141627,-68.1554246256358));
#17631=CARTESIAN_POINT('Ctrl Pts',(-79.8655136998482,150.071648626446,-68.2052448161789));
#17632=CARTESIAN_POINT('Ctrl Pts',(-79.7739999236149,150.120350661883,-68.3371509124479));
#17633=CARTESIAN_POINT('Ctrl Pts',(-79.6818941936877,150.16926027239,-68.46839508031));
#17634=CARTESIAN_POINT('Ctrl Pts',(-79.5892012521672,150.218371135719,-68.5989889747242));
#17635=CARTESIAN_POINT('Ctrl Pts',(-79.3779141702089,150.330315916359,-68.8966686299355));
#17636=CARTESIAN_POINT('Ctrl Pts',(-79.163579340244,150.443304640525,-69.1909515362395));
#17637=CARTESIAN_POINT('Ctrl Pts',(-78.9462744635298,150.557250733189,-69.4819552440033));
#17638=CARTESIAN_POINT('Ctrl Pts',(-78.484031024483,150.799632931579,-70.1009682946354));
#17639=CARTESIAN_POINT('Ctrl Pts',(-78.0084220634587,151.04629879067,-70.7052523960841));
#17640=CARTESIAN_POINT('Ctrl Pts',(-77.5199570397094,151.296570144028,-71.2955928713244));
#17641=CARTESIAN_POINT('Ctrl Pts',(-77.0216110413805,151.55190414212,-71.8978751211965));
#17642=CARTESIAN_POINT('Ctrl Pts',(-76.5098835991764,151.810990946169,-72.4856440211327));
#17643=CARTESIAN_POINT('Ctrl Pts',(-75.9853380432724,152.073093135985,-73.0597795388602));
#17644=CARTESIAN_POINT('Ctrl Pts',(-75.9066252473747,152.112423935644,-73.1459337561934));
#17645=CARTESIAN_POINT('Ctrl Pts',(-75.827623857029,152.151822604378,-73.23178106206));
#17646=CARTESIAN_POINT('Ctrl Pts',(-75.7483358179058,152.19128661854,-73.3173245146471));
#17647=CARTESIAN_POINT('Ctrl Pts',(-75.4824265393875,152.323637571463,-73.6042126507511));
#17648=CARTESIAN_POINT('Ctrl Pts',(-75.2132781171718,152.456731033711,-73.8876629525089));
#17649=CARTESIAN_POINT('Ctrl Pts',(-74.9409623838955,152.590472038921,-74.1677942224948));
#17650=CARTESIAN_POINT('Ctrl Pts',(-74.3167866632673,152.897020203802,-74.8098839585897));
#17651=CARTESIAN_POINT('Ctrl Pts',(-73.6759323983567,153.206997438947,-75.4344770901284));
#17652=CARTESIAN_POINT('Ctrl Pts',(-73.0188468713402,153.519527171665,-76.0423970896734));
#17653=CARTESIAN_POINT('Ctrl Pts',(-72.4866598929599,153.772651380418,-76.5347639039658));
#17654=CARTESIAN_POINT('Ctrl Pts',(-71.9438260409974,154.027449586919,-77.0161946043035));
#17655=CARTESIAN_POINT('Ctrl Pts',(-71.390591833358,154.283447572611,-77.4871484354879));
#17656=CARTESIAN_POINT('Ctrl Pts',(-71.0824660574145,154.426026568798,-77.7494478606924));
#17657=CARTESIAN_POINT('Ctrl Pts',(-70.7712601794406,154.568910483264,-78.0083517875374));
#17658=CARTESIAN_POINT('Ctrl Pts',(-70.4568502021148,154.712094742454,-78.2640882514698));
#17659=CARTESIAN_POINT('Ctrl Pts',(-70.0593478034779,154.893119807115,-78.5874108721342));
#17660=CARTESIAN_POINT('Ctrl Pts',(-69.6561647078897,155.074868533276,-78.9060258939702));
#17661=CARTESIAN_POINT('Ctrl Pts',(-69.248163363783,155.256846802623,-79.2194748965191));
#17662=CARTESIAN_POINT('Ctrl Pts',(-69.1753983116225,155.289301740462,-79.2753769991704));
#17663=CARTESIAN_POINT('Ctrl Pts',(-69.1024799874813,155.321763950337,-79.3311146571456));
#17664=CARTESIAN_POINT('Ctrl Pts',(-69.0294132721225,155.354230585197,-79.3866850949249));
#17665=CARTESIAN_POINT('Ctrl Pts',(-68.7054569495941,155.498178093751,-79.6330680693873));
#17666=CARTESIAN_POINT('Ctrl Pts',(-68.3790872245564,155.64198899673,-79.8757795810431));
#17667=CARTESIAN_POINT('Ctrl Pts',(-68.0508366323766,155.785376828615,-80.1145376578703));
#17668=CARTESIAN_POINT('Ctrl Pts',(-67.5615807059302,155.999095701336,-80.470405421273));
#17669=CARTESIAN_POINT('Ctrl Pts',(-67.0679849322336,156.211965564659,-80.8177011119818));
#17670=CARTESIAN_POINT('Ctrl Pts',(-66.5698782490513,156.423946748387,-81.1570290898547));
#17671=CARTESIAN_POINT('Ctrl Pts',(-66.2383201338304,156.565049215211,-81.3828982632343));
#17672=CARTESIAN_POINT('Ctrl Pts',(-65.9048194379772,156.705733562974,-81.6051889022944));
#17673=CARTESIAN_POINT('Ctrl Pts',(-65.5694149143534,156.845949350922,-81.8240186527302));
#17674=CARTESIAN_POINT('Ctrl Pts',(-64.6829201703191,157.216548285317,-82.4023991155329));
#17675=CARTESIAN_POINT('Ctrl Pts',(-63.7831508540726,157.583856508053,-82.9566758456117));
#17676=CARTESIAN_POINT('Ctrl Pts',(-62.8706182035639,157.947089454461,-83.4884243400324));
#17677=CARTESIAN_POINT('Ctrl Pts',(-62.3950459017896,158.136390657335,-83.7655485123189));
#17678=CARTESIAN_POINT('Ctrl Pts',(-61.9160072268454,158.324584912065,-84.0365547854392));
#17679=CARTESIAN_POINT('Ctrl Pts',(-61.4335758366808,158.511560631034,-84.3016715534536));
#17680=CARTESIAN_POINT('Ctrl Pts',(-61.0961749032255,158.642326960506,-84.4870878568419));
#17681=CARTESIAN_POINT('Ctrl Pts',(-60.7571134074066,158.772497700688,-84.6696164130183));
#17682=CARTESIAN_POINT('Ctrl Pts',(-60.4164146176901,158.902035370161,-84.8493358861248));
#17683=CARTESIAN_POINT('Ctrl Pts',(-59.3438850557613,159.309823669053,-85.4150979421665));
#17684=CARTESIAN_POINT('Ctrl Pts',(-58.2551149681582,159.711350535676,-85.9529757040515));
#17685=CARTESIAN_POINT('Ctrl Pts',(-57.1505460201433,160.105633614135,-86.4645921180823));
#17686=CARTESIAN_POINT('Ctrl Pts',(-56.4487513530865,160.356143790318,-86.7896507498597));
#17687=CARTESIAN_POINT('Ctrl Pts',(-55.7405793567733,160.603729602651,-87.1041092869249));
#17688=CARTESIAN_POINT('Ctrl Pts',(-55.0261465205371,160.84813707073,-87.4083941820344));
#17689=CARTESIAN_POINT('Ctrl Pts',(-53.8092543837208,161.264435861881,-87.9266820845914));
#17690=CARTESIAN_POINT('Ctrl Pts',(-52.5741889959425,161.671522365092,-88.415424491364));
#17691=CARTESIAN_POINT('Ctrl Pts',(-51.321279392281,162.068275297191,-88.8760332304436));
#17692=CARTESIAN_POINT('Ctrl Pts',(-51.0020471261459,162.169365062358,-88.9933929913939));
#17693=CARTESIAN_POINT('Ctrl Pts',(-50.6816565051252,162.269783934374,-89.1089265816755));
#17694=CARTESIAN_POINT('Ctrl Pts',(-50.3601131347592,162.369513278003,-89.2226578573149));
#17695=CARTESIAN_POINT('Ctrl Pts',(-50.0449901630546,162.467251281727,-89.3341182102819));
#17696=CARTESIAN_POINT('Ctrl Pts',(-49.7287558621685,162.564328303438,-89.4438470825149));
#17697=CARTESIAN_POINT('Ctrl Pts',(-49.4114172566784,162.660726190096,-89.5518664732));
#17698=CARTESIAN_POINT('Ctrl Pts',(-48.5859802317114,162.911469035119,-89.8328382898754));
#17699=CARTESIAN_POINT('Ctrl Pts',(-47.7517061842026,163.15799803978,-90.1026104418408));
#17700=CARTESIAN_POINT('Ctrl Pts',(-46.9134264693539,163.398683586024,-90.3600730618877));
#17701=CARTESIAN_POINT('Ctrl Pts',(-46.7837842030723,163.435906268529,-90.3998903650557));
#17702=CARTESIAN_POINT('Ctrl Pts',(-46.6540462294582,163.47298916605,-90.4394132489993));
#17703=CARTESIAN_POINT('Ctrl Pts',(-46.5242305246109,163.509926224964,-90.4786376019946));
#17704=CARTESIAN_POINT('Ctrl Pts',(-45.8392025345838,163.704840386199,-90.6856216469843));
#17705=CARTESIAN_POINT('Ctrl Pts',(-45.1519736911824,163.89572719544,-90.8843501937075));
#17706=CARTESIAN_POINT('Ctrl Pts',(-44.4626074592405,164.082529655127,-91.0751334104582));
#17707=CARTESIAN_POINT('Ctrl Pts',(-44.1783869467075,164.159546904268,-91.153791895796));
#17708=CARTESIAN_POINT('Ctrl Pts',(-43.893801405373,164.235870359354,-91.2310993615674));
#17709=CARTESIAN_POINT('Ctrl Pts',(-43.608853696462,164.311496491514,-91.3070783228867));
#17710=CARTESIAN_POINT('Ctrl Pts',(-42.1660734698655,164.69441547869,-91.6917837955071));
#17711=CARTESIAN_POINT('Ctrl Pts',(-40.7140157437857,165.059455982243,-92.0424908351377));
#17712=CARTESIAN_POINT('Ctrl Pts',(-39.2529743664741,165.406179164334,-92.3614696565619));
#17713=CARTESIAN_POINT('Ctrl Pts',(-38.9827628953543,165.47030368713,-92.4204630142665));
#17714=CARTESIAN_POINT('Ctrl Pts',(-38.7122441503414,165.533801695374,-92.4783712680377));
#17715=CARTESIAN_POINT('Ctrl Pts',(-38.4414200000023,165.596670438918,-92.5352089701923));
#17716=CARTESIAN_POINT('Ctrl Pts',(-38.2001914433258,165.652668902299,-92.5858354628386));
#17717=CARTESIAN_POINT('Ctrl Pts',(-37.9587206663411,165.708168099145,-92.6356114700981));
#17718=CARTESIAN_POINT('Ctrl Pts',(-37.7170088289231,165.763166128676,-92.6845472946188));
#17719=CARTESIAN_POINT('Ctrl Pts',(-36.0211739040145,166.14902881656,-93.0278779365432));
#17720=CARTESIAN_POINT('Ctrl Pts',(-34.3135008475802,166.510233714585,-93.3300633545587));
#17721=CARTESIAN_POINT('Ctrl Pts',(-32.5942104457704,166.846108960576,-93.5932011303994));
#17722=CARTESIAN_POINT('Ctrl Pts',(-30.8504021259006,167.186773951074,-93.8600913790159));
#17723=CARTESIAN_POINT('Ctrl Pts',(-29.094642715236,167.501381720967,-94.0868124355136));
#17724=CARTESIAN_POINT('Ctrl Pts',(-27.3271657460881,167.789235416743,-94.27560615426));
#17725=CARTESIAN_POINT('Ctrl Pts',(-26.91682780789,167.856063609749,-94.319436555814));
#17726=CARTESIAN_POINT('Ctrl Pts',(-26.505858326992,167.921449818373,-94.3612229556582));
#17727=CARTESIAN_POINT('Ctrl Pts',(-26.0942602532882,167.985385353875,-94.4009938026451));
#17728=CARTESIAN_POINT('Ctrl Pts',(-25.9629814123699,168.005777536275,-94.4136786790533));
#17729=CARTESIAN_POINT('Ctrl Pts',(-25.8316384428103,168.02602217232,-94.4261573441815));
#17730=CARTESIAN_POINT('Ctrl Pts',(-25.7002314412141,168.046118978926,-94.4384308363077));
#17731=CARTESIAN_POINT('Ctrl Pts',(-23.7387849731355,168.346093941119,-94.6216311033371));
#17732=CARTESIAN_POINT('Ctrl Pts',(-21.7630551046537,168.613150513186,-94.7590226613957));
#17733=CARTESIAN_POINT('Ctrl Pts',(-19.7730895732306,168.846191178979,-94.8521329477807));
#17734=CARTESIAN_POINT('Ctrl Pts',(-18.7114479901565,168.970517785369,-94.9018070503103));
#17735=CARTESIAN_POINT('Ctrl Pts',(-17.6478952698206,169.084909038081,-94.9387840850485));
#17736=CARTESIAN_POINT('Ctrl Pts',(-16.5829228051783,169.189282687295,-94.9633322911818));
#17737=CARTESIAN_POINT('Ctrl Pts',(-15.517950340536,169.29365633651,-94.9878804973151));
#17738=CARTESIAN_POINT('Ctrl Pts',(-14.4515581849858,169.388012296297,-95.));
#17739=CARTESIAN_POINT('Ctrl Pts',(-13.3842538190364,169.472303783561,-95.));
#17740=CARTESIAN_POINT('',(60.1292596944771,159.010918268508,-95.));
#17741=CARTESIAN_POINT('Origin',(0.,0.,-95.));
#17742=CARTESIAN_POINT('Ctrl Pts',(60.1292596944771,159.010918268508,-95.));
#17743=CARTESIAN_POINT('Ctrl Pts',(64.3119987470806,157.429234410148,-95.));
#17744=CARTESIAN_POINT('Ctrl Pts',(68.3990993783209,155.695446906751,-94.8693321132271));
#17745=CARTESIAN_POINT('Ctrl Pts',(76.3918383640665,151.93352498582,-94.391839127194));
#17746=CARTESIAN_POINT('Ctrl Pts',(80.2974374490313,149.90536162208,-94.0447751990941));
#17747=CARTESIAN_POINT('Ctrl Pts',(87.9320651786579,145.558400023304,-93.1636543714777));
#17748=CARTESIAN_POINT('Ctrl Pts',(91.6610773848025,143.239594513987,-92.629470733653));
#17749=CARTESIAN_POINT('Ctrl Pts',(97.1228487062774,139.542057800314,-91.7023378918564));
#17750=CARTESIAN_POINT('Ctrl Pts',(98.9214514964918,138.272948251204,-91.372249811654));
#17751=CARTESIAN_POINT('Ctrl Pts',(102.474445246975,135.660789676228,-90.6717003069366));
#17752=CARTESIAN_POINT('Ctrl Pts',(104.218656939756,134.325187322145,-90.3032328616472));
#17753=CARTESIAN_POINT('Ctrl Pts',(109.350986406493,130.236321299975,-89.1485001127697));
#17754=CARTESIAN_POINT('Ctrl Pts',(112.641800518645,127.399064480377,-88.3125351604413));
#17755=CARTESIAN_POINT('Ctrl Pts',(118.972801758344,121.507898082088,-86.5241909359486));
#17756=CARTESIAN_POINT('Ctrl Pts',(122.012955421471,118.453972784964,-85.5717532843836));
#17757=CARTESIAN_POINT('Ctrl Pts',(127.847768104756,112.131410184014,-83.5609410285741));
#17758=CARTESIAN_POINT('Ctrl Pts',(130.642414202373,108.862770163068,-82.5025330088399));
#17759=CARTESIAN_POINT('Ctrl Pts',(133.982415980692,104.641632024445,-81.1174384551523));
#17760=CARTESIAN_POINT('Ctrl Pts',(134.642739315732,103.790628244652,-80.8373069772816));
#17761=CARTESIAN_POINT('Ctrl Pts',(135.947988660783,102.075002527314,-80.270890996809));
#17762=CARTESIAN_POINT('Ctrl Pts',(136.593106061479,101.210081480818,-79.9845055141404));
#17763=CARTESIAN_POINT('Ctrl Pts',(138.4979580987,98.604992114986,-79.1196138720762));
#17764=CARTESIAN_POINT('Ctrl Pts',(139.729721387279,96.8512586573184,-78.5343105220887));
#17765=CARTESIAN_POINT('Ctrl Pts',(145.702278354011,87.9990202333266,-75.566758076221));
#17766=CARTESIAN_POINT('Ctrl Pts',(149.887796395751,80.6511722105745,-73.062763378222));
#17767=CARTESIAN_POINT('Ctrl Pts',(155.317122432713,69.2411167663415,-69.1413436830464));
#17768=CARTESIAN_POINT('Ctrl Pts',(156.984715626498,65.3727814509462,-67.8063628366596));
#17769=CARTESIAN_POINT('Ctrl Pts',(159.271963035734,59.4717762008594,-65.7638052213179));
#17770=CARTESIAN_POINT('Ctrl Pts',(159.998649543538,57.488341079772,-65.0762597501037));
#17771=CARTESIAN_POINT('Ctrl Pts',(161.034620693271,54.4882578372571,-64.0350107773724));
#17772=CARTESIAN_POINT('Ctrl Pts',(161.371184461829,53.4832599490673,-63.6859889324587));
#17773=CARTESIAN_POINT('Ctrl Pts',(162.024054573491,51.4715844807547,-62.9869704073305));
#17774=CARTESIAN_POINT('Ctrl Pts',(162.340565299031,50.4643653454645,-62.6367861123213));
#17775=CARTESIAN_POINT('Ctrl Pts',(165.100688409562,41.3870343438974,-59.4792352470941));
#17776=CARTESIAN_POINT('Ctrl Pts',(166.928575054619,33.2308356969195,-56.6310812172013));
#17777=CARTESIAN_POINT('Ctrl Pts',(168.765868892532,20.8672206982357,-52.3070906459483));
#17778=CARTESIAN_POINT('Ctrl Pts',(169.226876637901,16.7243838271306,-50.8570487361151));
#17779=CARTESIAN_POINT('Ctrl Pts',(169.689684284876,10.477177341883,-48.6696274303821));
#17780=CARTESIAN_POINT('Ctrl Pts',(169.805796892358,8.38927803590911,-47.9384240498734));
#17781=CARTESIAN_POINT('Ctrl Pts',(169.922171669824,5.24907001896995,-46.8385881425543));
#17782=CARTESIAN_POINT('Ctrl Pts',(169.965906660215,3.67687569683897,-46.2879122489256));
#17783=CARTESIAN_POINT('Ctrl Pts',(169.991474952794,1.8389601147623,-45.6441423007187));
#17784=CARTESIAN_POINT('Ctrl Pts',(169.996957619285,1.05048782907507,-45.3679602834514));
#17785=CARTESIAN_POINT('Ctrl Pts',(169.999393685716,0.524662730744418,-45.1837767020228));
#17786=CARTESIAN_POINT('Ctrl Pts',(170.,0.260336526753546,-45.091189605798));
#17787=CARTESIAN_POINT('Ctrl Pts',(170.,0.,-45.));
#17788=CARTESIAN_POINT('',(145.36231884058,-88.1464478086873,-32.5));
#17789=CARTESIAN_POINT('Origin',(0.,0.,-32.5));
#17790=CARTESIAN_POINT('',(150.289855072464,-79.4541343310581,-37.5));
#17791=CARTESIAN_POINT('Ctrl Pts',(145.36231884058,-88.1464478086873,-32.5));
#17792=CARTESIAN_POINT('Ctrl Pts',(145.729245618505,-87.5413488102603,-32.5000000006552));
#17793=CARTESIAN_POINT('Ctrl Pts',(146.089427518266,-86.9388521048938,-32.5405483747626));
#17794=CARTESIAN_POINT('Ctrl Pts',(146.443059039059,-86.3390436926112,-32.6214654834413));
#17795=CARTESIAN_POINT('Ctrl Pts',(146.591729838526,-86.0868772681335,-32.6554839759412));
#17796=CARTESIAN_POINT('Ctrl Pts',(146.739242777582,-85.8351860206267,-32.6966381016031));
#17797=CARTESIAN_POINT('Ctrl Pts',(146.885611849037,-85.5839764893768,-32.744917216543));
#17798=CARTESIAN_POINT('Ctrl Pts',(146.887215711036,-85.5812238216389,-32.7454462424977));
#17799=CARTESIAN_POINT('Ctrl Pts',(146.888819435246,-85.578471212414,-32.745976138191));
#17800=CARTESIAN_POINT('Ctrl Pts',(146.890423021642,-85.5757186617923,-32.7465069043789));
#17801=CARTESIAN_POINT('Ctrl Pts',(147.136163003217,-85.1539068149984,-32.8278436340878));
#17802=CARTESIAN_POINT('Ctrl Pts',(147.378654044698,-84.7334926273371,-32.9296159558605));
#17803=CARTESIAN_POINT('Ctrl Pts',(147.617771548819,-84.3148475830954,-33.0545296220188));
#17804=CARTESIAN_POINT('Ctrl Pts',(147.619992196193,-84.3109596911514,-33.0556896759668));
#17805=CARTESIAN_POINT('Ctrl Pts',(147.622212556282,-84.307071941363,-33.0568517414269));
#17806=CARTESIAN_POINT('Ctrl Pts',(147.624432625828,-84.303184339794,-33.0580158203818));
#17807=CARTESIAN_POINT('Ctrl Pts',(147.797445356378,-84.0002188025685,-33.1487339147363));
#17808=CARTESIAN_POINT('Ctrl Pts',(147.968707325063,-83.6981287773935,-33.2516890850514));
#17809=CARTESIAN_POINT('Ctrl Pts',(148.136615102467,-83.3998939040528,-33.3677714304339));
#17810=CARTESIAN_POINT('Ctrl Pts',(148.200188499827,-83.2869759415708,-33.4117226349792));
#17811=CARTESIAN_POINT('Ctrl Pts',(148.263281189286,-83.1746104687379,-33.4575552147659));
#17812=CARTESIAN_POINT('Ctrl Pts',(148.325806750806,-83.0629583612556,-33.505315729073));
#17813=CARTESIAN_POINT('Ctrl Pts',(148.328437712999,-83.0582602431351,-33.5073254048666));
#17814=CARTESIAN_POINT('Ctrl Pts',(148.331067922545,-83.0535629380491,-33.5093386477995));
#17815=CARTESIAN_POINT('Ctrl Pts',(148.333697371915,-83.0488664605802,-33.5113554669624));
#17816=CARTESIAN_POINT('Ctrl Pts',(148.479392264039,-82.7886398192674,-33.6231051943638));
#17817=CARTESIAN_POINT('Ctrl Pts',(148.622808980514,-82.5308543501899,-33.7458732653459));
#17818=CARTESIAN_POINT('Ctrl Pts',(148.762663380364,-82.2779954794438,-33.8812204176226));
#17819=CARTESIAN_POINT('Ctrl Pts',(148.840976562993,-82.1364040604732,-33.9570097118165));
#17820=CARTESIAN_POINT('Ctrl Pts',(148.918172933482,-81.9963571593236,-34.0367425583452));
#17821=CARTESIAN_POINT('Ctrl Pts',(148.994029023493,-81.858288006606,-34.1206866444586));
#17822=CARTESIAN_POINT('Ctrl Pts',(148.996712266486,-81.8534041128196,-34.1236559825947));
#17823=CARTESIAN_POINT('Ctrl Pts',(148.999393672824,-81.8485229853464,-34.1266302098562));
#17824=CARTESIAN_POINT('Ctrl Pts',(149.002073232326,-81.8436446453384,-34.1296093604689));
#17825=CARTESIAN_POINT('Ctrl Pts',(149.107681065301,-81.6513776267186,-34.24702479387));
#17826=CARTESIAN_POINT('Ctrl Pts',(149.210443318176,-81.4633981454561,-34.3720951240627));
#17827=CARTESIAN_POINT('Ctrl Pts',(149.309720948425,-81.2810297213995,-34.5068954514884));
#17828=CARTESIAN_POINT('Ctrl Pts',(149.401996349968,-81.1115240682479,-34.6321880708852));
#17829=CARTESIAN_POINT('Ctrl Pts',(149.491261252783,-80.9468661109974,-34.7658868965042));
#17830=CARTESIAN_POINT('Ctrl Pts',(149.577013895292,-80.7880986855831,-34.9096181572236));
#17831=CARTESIAN_POINT('Ctrl Pts',(149.5835211508,-80.7760507746002,-34.9205250635371));
#17832=CARTESIAN_POINT('Ctrl Pts',(149.590008187532,-80.7640367724579,-34.9314897186423));
#17833=CARTESIAN_POINT('Ctrl Pts',(149.596474789369,-80.7520571291769,-34.94251282205));
#17834=CARTESIAN_POINT('Ctrl Pts',(149.598641974416,-80.7480423306098,-34.9462070505615));
#17835=CARTESIAN_POINT('Ctrl Pts',(149.600807137209,-80.7440308818108,-34.9499087160619));
#17836=CARTESIAN_POINT('Ctrl Pts',(149.602970226706,-80.7400228807505,-34.9536178068362));
#17837=CARTESIAN_POINT('Ctrl Pts',(149.665071318773,-80.6249554074952,-35.0601037326242));
#17838=CARTESIAN_POINT('Ctrl Pts',(149.72550324979,-80.5126559823695,-35.1727795475935));
#17839=CARTESIAN_POINT('Ctrl Pts',(149.783030801438,-80.4054929784085,-35.2913281843215));
#17840=CARTESIAN_POINT('Ctrl Pts',(149.809543927947,-80.3561040126055,-35.3459645266126));
#17841=CARTESIAN_POINT('Ctrl Pts',(149.835440369613,-80.3078056561145,-35.401847873638));
#17842=CARTESIAN_POINT('Ctrl Pts',(149.860600799429,-80.260826858674,-35.4589450748328));
#17843=CARTESIAN_POINT('Ctrl Pts',(149.862244464558,-80.2577578566055,-35.4626750857764));
#17844=CARTESIAN_POINT('Ctrl Pts',(149.863885113164,-80.2546942576159,-35.4664102868023));
#17845=CARTESIAN_POINT('Ctrl Pts',(149.865522721632,-80.2516361085806,-35.4701507147205));
#17846=CARTESIAN_POINT('Ctrl Pts',(149.920874283244,-80.1482699328262,-35.5965780814448));
#17847=CARTESIAN_POINT('Ctrl Pts',(149.972772946805,-80.0510921734565,-35.7290075001422));
#17848=CARTESIAN_POINT('Ctrl Pts',(150.020328326758,-79.9618719405058,-35.8689218234402));
#17849=CARTESIAN_POINT('Ctrl Pts',(150.04142343791,-79.92229469955,-35.9309864774229));
#17850=CARTESIAN_POINT('Ctrl Pts',(150.061664115497,-79.8842828909716,-35.9945234855749));
#17851=CARTESIAN_POINT('Ctrl Pts',(150.080973718749,-79.8479888765764,-36.0596598378906));
#17852=CARTESIAN_POINT('Ctrl Pts',(150.081910893431,-79.8462273783758,-36.0628211737006));
#17853=CARTESIAN_POINT('Ctrl Pts',(150.082845417364,-79.8444707888363,-36.0659847749909));
#17854=CARTESIAN_POINT('Ctrl Pts',(150.083777280819,-79.842719127427,-36.0691506505178));
#17855=CARTESIAN_POINT('Ctrl Pts',(150.124316972746,-79.766515029516,-36.2068785740439));
#17856=CARTESIAN_POINT('Ctrl Pts',(150.159836015383,-79.6996105779044,-36.3489635265317));
#17857=CARTESIAN_POINT('Ctrl Pts',(150.189536570947,-79.6436016305286,-36.4961016996745));
#17858=CARTESIAN_POINT('Ctrl Pts',(150.205994764959,-79.6125649679198,-36.5776364910011));
#17859=CARTESIAN_POINT('Ctrl Pts',(150.220666659912,-79.5848732537884,-36.6607227768373));
#17860=CARTESIAN_POINT('Ctrl Pts',(150.233419649245,-79.5607919801431,-36.7454773415068));
#17861=CARTESIAN_POINT('Ctrl Pts',(150.233653158554,-79.5603510481059,-36.747029211371));
#17862=CARTESIAN_POINT('Ctrl Pts',(150.233885994755,-79.5599113833124,-36.7485818022511));
#17863=CARTESIAN_POINT('Ctrl Pts',(150.234118156878,-79.5594729876405,-36.7501351076896));
#17864=CARTESIAN_POINT('Ctrl Pts',(150.243593980634,-79.541579629057,-36.8135341168033));
#17865=CARTESIAN_POINT('Ctrl Pts',(150.251930637624,-79.5258311439938,-36.8780113419661));
#17866=CARTESIAN_POINT('Ctrl Pts',(150.25908694937,-79.5123085902626,-36.9432880969468));
#17867=CARTESIAN_POINT('Ctrl Pts',(150.266133192885,-79.49899402126,-37.0075608575311));
#17868=CARTESIAN_POINT('Ctrl Pts',(150.272035277523,-79.4878371314995,-37.0726101138062));
#17869=CARTESIAN_POINT('Ctrl Pts',(150.276731655023,-79.4789572453976,-37.1381835195656));
#17870=CARTESIAN_POINT('Ctrl Pts',(150.281154338818,-79.4705948579247,-37.1999354632936));
#17871=CARTESIAN_POINT('Ctrl Pts',(150.284507727575,-79.4642518495709,-37.2621532653189));
#17872=CARTESIAN_POINT('Ctrl Pts',(150.286719886614,-79.4600667280323,-37.3246214692043));
#17873=CARTESIAN_POINT('Ctrl Pts',(150.28878458935,-79.4561605749315,-37.3829257182103));
#17874=CARTESIAN_POINT('Ctrl Pts',(150.289855072332,-79.4541343313065,-37.4414487162201));
#17875=CARTESIAN_POINT('Ctrl Pts',(150.289855072464,-79.4541343310581,-37.5));
#17876=CARTESIAN_POINT('',(150.289855072464,-79.4541343310581,-44.5));
#17877=CARTESIAN_POINT('',(150.289855072464,-79.4541343310581,115.));
#17878=CARTESIAN_POINT('',(145.36231884058,-88.1464478086873,-49.5));
#17879=CARTESIAN_POINT('Ctrl Pts',(150.289855072464,-79.4541343310581,-44.5));
#17880=CARTESIAN_POINT('Ctrl Pts',(150.289855068577,-79.4541343384106,-44.7563523801461));
#17881=CARTESIAN_POINT('Ctrl Pts',(150.270581238553,-79.4906188049207,-45.0053815220034));
#17882=CARTESIAN_POINT('Ctrl Pts',(150.23440031069,-79.5589401936918,-45.2480116426047));
#17883=CARTESIAN_POINT('Ctrl Pts',(150.233993766309,-79.5597078820386,-45.2507379384179));
#17884=CARTESIAN_POINT('Ctrl Pts',(150.2335850823,-79.5604795994257,-45.2534634549803));
#17885=CARTESIAN_POINT('Ctrl Pts',(150.233174261933,-79.5612553394204,-45.2561881931872));
#17886=CARTESIAN_POINT('Ctrl Pts',(150.211108362005,-79.6029217280976,-45.4025387770759));
#17887=CARTESIAN_POINT('Ctrl Pts',(150.183223768725,-79.6555340186023,-45.5439666089425));
#17888=CARTESIAN_POINT('Ctrl Pts',(150.1506572954,-79.7168744981717,-45.6800320781738));
#17889=CARTESIAN_POINT('Ctrl Pts',(150.129869982031,-79.7560283776325,-45.7668832247325));
#17890=CARTESIAN_POINT('Ctrl Pts',(150.107175698374,-79.7987372958143,-45.8515497663918));
#17891=CARTESIAN_POINT('Ctrl Pts',(150.082875014061,-79.8444151271613,-45.9339198071965));
#17892=CARTESIAN_POINT('Ctrl Pts',(150.081600916097,-79.8468100404567,-45.9382385127928));
#17893=CARTESIAN_POINT('Ctrl Pts',(150.080322360848,-79.8492131928944,-45.9425510499967));
#17894=CARTESIAN_POINT('Ctrl Pts',(150.079039391808,-79.8516244996445,-45.94685739874));
#17895=CARTESIAN_POINT('Ctrl Pts',(150.044542112121,-79.9164612343949,-46.0626492162668));
#17896=CARTESIAN_POINT('Ctrl Pts',(150.006537123161,-79.9877842271942,-46.1748654509807));
#17897=CARTESIAN_POINT('Ctrl Pts',(149.965970804575,-80.0637685565973,-46.2827346305569));
#17898=CARTESIAN_POINT('Ctrl Pts',(149.933351576217,-80.1248672778719,-46.3694718432009));
#17899=CARTESIAN_POINT('Ctrl Pts',(149.899077126141,-80.1889782570263,-46.4533984421142));
#17900=CARTESIAN_POINT('Ctrl Pts',(149.863649966461,-80.2551332464111,-46.5341227219249));
#17901=CARTESIAN_POINT('Ctrl Pts',(149.861515024356,-80.2591199355374,-46.5389873982183));
#17902=CARTESIAN_POINT('Ctrl Pts',(149.85937578758,-80.2631142503699,-46.5438407130638));
#17903=CARTESIAN_POINT('Ctrl Pts',(149.857232364154,-80.2671159825673,-46.5486825816028));
#17904=CARTESIAN_POINT('Ctrl Pts',(149.804252858279,-80.3660277477057,-46.6683601962307));
#17905=CARTESIAN_POINT('Ctrl Pts',(149.748484158479,-80.4699094430547,-46.7819066280769));
#17906=CARTESIAN_POINT('Ctrl Pts',(149.690355247898,-80.5778965450365,-46.8902500251402));
#17907=CARTESIAN_POINT('Ctrl Pts',(149.661473306408,-80.6315510369212,-46.9440815458665));
#17908=CARTESIAN_POINT('Ctrl Pts',(149.632008986731,-80.6862185045812,-46.9966292711324));
#17909=CARTESIAN_POINT('Ctrl Pts',(149.60201639041,-80.741790230842,-47.0480105076949));
#17910=CARTESIAN_POINT('Ctrl Pts',(149.599223408299,-80.7469652025476,-47.0527952510041));
#17911=CARTESIAN_POINT('Ctrl Pts',(149.596425806469,-80.7521480873936,-47.0575699305601));
#17912=CARTESIAN_POINT('Ctrl Pts',(149.593623625112,-80.7573388040449,-47.0623346471253));
#17913=CARTESIAN_POINT('Ctrl Pts',(149.503321107799,-80.9246137661054,-47.2158814184506));
#17914=CARTESIAN_POINT('Ctrl Pts',(149.407759531995,-81.1009468141059,-47.3595995786781));
#17915=CARTESIAN_POINT('Ctrl Pts',(149.309404815745,-81.2816192446479,-47.4931449450858));
#17916=CARTESIAN_POINT('Ctrl Pts',(149.306147321137,-81.2876030905749,-47.4975679491626));
#17917=CARTESIAN_POINT('Ctrl Pts',(149.302886794892,-81.2935916372183,-47.501979751875));
#17918=CARTESIAN_POINT('Ctrl Pts',(149.299623326396,-81.2995847135535,-47.5063803428043));
#17919=CARTESIAN_POINT('Ctrl Pts',(149.201294060241,-81.4801578671638,-47.6389714425028));
#17920=CARTESIAN_POINT('Ctrl Pts',(149.100390942177,-81.6646756184357,-47.7614147349028));
#17921=CARTESIAN_POINT('Ctrl Pts',(148.997297013874,-81.8523394986245,-47.8757113225169));
#17922=CARTESIAN_POINT('Ctrl Pts',(148.993783486671,-81.8587352404397,-47.8796066457086));
#17923=CARTESIAN_POINT('Ctrl Pts',(148.99026742009,-81.8651346268366,-47.8834924864782));
#17924=CARTESIAN_POINT('Ctrl Pts',(148.986748829868,-81.871537625153,-47.8873689234621));
#17925=CARTESIAN_POINT('Ctrl Pts',(148.828989572841,-82.1586219951734,-48.0611725720732));
#17926=CARTESIAN_POINT('Ctrl Pts',(148.666197518726,-82.4528887104789,-48.2162655070009));
#17927=CARTESIAN_POINT('Ctrl Pts',(148.499047675041,-82.7528397905676,-48.3561560144813));
#17928=CARTESIAN_POINT('Ctrl Pts',(148.443888606593,-82.851822965143,-48.4023195639484));
#17929=CARTESIAN_POINT('Ctrl Pts',(148.388255039765,-82.9514250577883,-48.4468280100297));
#17930=CARTESIAN_POINT('Ctrl Pts',(148.332171389768,-83.0515919680528,-48.4898085924912));
#17931=CARTESIAN_POINT('Ctrl Pts',(148.328463625565,-83.0582141348388,-48.4926500955871));
#17932=CARTESIAN_POINT('Ctrl Pts',(148.324753888106,-83.0648387811285,-48.4954849142925));
#17933=CARTESIAN_POINT('Ctrl Pts',(148.321042184227,-83.0714658916725,-48.4983130852896));
#17934=CARTESIAN_POINT('Ctrl Pts',(148.127526079489,-83.4169817679216,-48.6457646742983));
#17935=CARTESIAN_POINT('Ctrl Pts',(147.928023779063,-83.7703038873281,-48.7751050652708));
#17936=CARTESIAN_POINT('Ctrl Pts',(147.726117191241,-84.1248695147338,-48.8871259760477));
#17937=CARTESIAN_POINT('Ctrl Pts',(147.691851026851,-84.1850438963965,-48.9061373762463));
#17938=CARTESIAN_POINT('Ctrl Pts',(147.657515670427,-84.2452539899323,-48.9246499566981));
#17939=CARTESIAN_POINT('Ctrl Pts',(147.623128700903,-84.3054675885421,-48.9426676169133));
#17940=CARTESIAN_POINT('Ctrl Pts',(147.61966084937,-84.3115399997817,-48.9444846589923));
#17941=CARTESIAN_POINT('Ctrl Pts',(147.616192453019,-84.3176124815105,-48.9462966777585));
#17942=CARTESIAN_POINT('Ctrl Pts',(147.612723530195,-84.3236850001122,-48.9481036768601));
#17943=CARTESIAN_POINT('Ctrl Pts',(147.41439805748,-84.6708634135425,-49.0514135425518));
#17944=CARTESIAN_POINT('Ctrl Pts',(147.213653682834,-85.0194306321946,-49.1388789349076));
#17945=CARTESIAN_POINT('Ctrl Pts',(147.010609976465,-85.3690841855301,-49.211977417735));
#17946=CARTESIAN_POINT('Ctrl Pts',(146.970506380402,-85.4381450055664,-49.2264152551867));
#17947=CARTESIAN_POINT('Ctrl Pts',(146.930313102763,-85.5072481940793,-49.2402927866165));
#17948=CARTESIAN_POINT('Ctrl Pts',(146.89003109062,-85.5763914060563,-49.253621628096));
#17949=CARTESIAN_POINT('Ctrl Pts',(146.887290932544,-85.5810948287668,-49.254528314001));
#17950=CARTESIAN_POINT('Ctrl Pts',(146.884550362083,-85.5857984397406,-49.2554324609279));
#17951=CARTESIAN_POINT('Ctrl Pts',(146.881809379355,-85.5905022385503,-49.2563340725845));
#17952=CARTESIAN_POINT('Ctrl Pts',(146.534412670951,-86.18666952076,-49.3706058330548));
#17953=CARTESIAN_POINT('Ctrl Pts',(146.180413916078,-86.7858240349752,-49.4448187829498));
#17954=CARTESIAN_POINT('Ctrl Pts',(145.819603406779,-87.3878896744197,-49.4786922813549));
#17955=CARTESIAN_POINT('Ctrl Pts',(145.668377265966,-87.6402328319036,-49.4928896461978));
#17956=CARTESIAN_POINT('Ctrl Pts',(145.515954394526,-87.8930873961788,-49.4999999997319));
#17957=CARTESIAN_POINT('Ctrl Pts',(145.36231884058,-88.1464478086873,-49.5));
#17958=CARTESIAN_POINT('Origin',(0.,0.,-49.5));
#17959=CARTESIAN_POINT('',(114.505594583524,-125.652173913043,-87.5));
#17960=CARTESIAN_POINT('Ctrl Pts',(114.505594583524,-125.652173913043,-87.5));
#17961=CARTESIAN_POINT('Ctrl Pts',(114.875320875519,-125.315245966795,-87.4999999999648));
#17962=CARTESIAN_POINT('Ctrl Pts',(115.240344836351,-124.979614106079,-87.4659613711684));
#17963=CARTESIAN_POINT('Ctrl Pts',(115.600645995236,-124.645458529299,-87.3949999533009));
#17964=CARTESIAN_POINT('Ctrl Pts',(115.815592867061,-124.44610947321,-87.3526661044782));
#17965=CARTESIAN_POINT('Ctrl Pts',(116.028858889205,-124.247285601145,-87.2971925568625));
#17966=CARTESIAN_POINT('Ctrl Pts',(116.240439697972,-124.049023288465,-87.2279752537402));
#17967=CARTESIAN_POINT('Ctrl Pts',(116.245828883255,-124.043973339257,-87.2262122163766));
#17968=CARTESIAN_POINT('Ctrl Pts',(116.251215926061,-124.038924730883,-87.2244403150212));
#17969=CARTESIAN_POINT('Ctrl Pts',(116.25660079453,-124.033877495354,-87.2226595463956));
#17970=CARTESIAN_POINT('Ctrl Pts',(116.416321748786,-123.884171095005,-87.1698400456397));
#17971=CARTESIAN_POINT('Ctrl Pts',(116.574127437902,-123.735675042354,-87.1092235237401));
#17972=CARTESIAN_POINT('Ctrl Pts',(116.729307011656,-123.58910958441,-87.0406588494489));
#17973=CARTESIAN_POINT('Ctrl Pts',(116.845631220437,-123.479242605673,-86.9892620625242));
#17974=CARTESIAN_POINT('Ctrl Pts',(116.960479920625,-123.37046021929,-86.9333980876332));
#17975=CARTESIAN_POINT('Ctrl Pts',(117.073550031386,-123.263067798316,-86.8729844025496));
#17976=CARTESIAN_POINT('Ctrl Pts',(117.079344844514,-123.257563965281,-86.8698882172442));
#17977=CARTESIAN_POINT('Ctrl Pts',(117.085135613102,-123.252063194138,-86.866779947454));
#17978=CARTESIAN_POINT('Ctrl Pts',(117.090922329314,-123.24656549557,-86.8636595351634));
#17979=CARTESIAN_POINT('Ctrl Pts',(117.252833947858,-123.09274055571,-86.7763507773278));
#17980=CARTESIAN_POINT('Ctrl Pts',(117.411527264105,-122.941364416115,-86.6795632238425));
#17981=CARTESIAN_POINT('Ctrl Pts',(117.566613453642,-122.792879292936,-86.5721870844575));
#17982=CARTESIAN_POINT('Ctrl Pts',(117.663683594909,-122.699940831258,-86.5049791850956));
#17983=CARTESIAN_POINT('Ctrl Pts',(117.759340859083,-122.608134753005,-86.4336238696905));
#17984=CARTESIAN_POINT('Ctrl Pts',(117.853493006743,-122.517566847009,-86.3578587588989));
#17985=CARTESIAN_POINT('Ctrl Pts',(117.859134880481,-122.512139751579,-86.3533186905155));
#17986=CARTESIAN_POINT('Ctrl Pts',(117.864772463519,-122.506716022107,-86.3487614273767));
#17987=CARTESIAN_POINT('Ctrl Pts',(117.870405487109,-122.50129592327,-86.3441871089973));
#17988=CARTESIAN_POINT('Ctrl Pts',(117.971986956638,-122.403554169479,-86.2616974876356));
#17989=CARTESIAN_POINT('Ctrl Pts',(118.072186599589,-122.30689585151,-86.1735699087614));
#17990=CARTESIAN_POINT('Ctrl Pts',(118.169344470473,-122.212953361586,-86.0806804467523));
#17991=CARTESIAN_POINT('Ctrl Pts',(118.186308138285,-122.196551096098,-86.064462038893));
#17992=CARTESIAN_POINT('Ctrl Pts',(118.203179139124,-122.180231567867,-86.0480985649969));
#17993=CARTESIAN_POINT('Ctrl Pts',(118.219948731942,-122.164003379953,-86.031594805261));
#17994=CARTESIAN_POINT('Ctrl Pts',(118.225239204071,-122.158883710274,-86.0263881981678));
#17995=CARTESIAN_POINT('Ctrl Pts',(118.2305200644,-122.153772676115,-86.0211674735436));
#17996=CARTESIAN_POINT('Ctrl Pts',(118.235791265575,-122.148670330441,-86.0159325934032));
#17997=CARTESIAN_POINT('Ctrl Pts',(118.348386205055,-122.039682211169,-85.9041134855647));
#17998=CARTESIAN_POINT('Ctrl Pts',(118.456626331103,-121.93460772812,-85.7857889099975));
#17999=CARTESIAN_POINT('Ctrl Pts',(118.560193282322,-121.833823583021,-85.6604137446068));
#18000=CARTESIAN_POINT('Ctrl Pts',(118.564867100718,-121.829275348417,-85.6547557547995));
#18001=CARTESIAN_POINT('Ctrl Pts',(118.569531415015,-121.824735838064,-85.649083428181));
#18002=CARTESIAN_POINT('Ctrl Pts',(118.57418617698,-121.820205105343,-85.6433966843365));
#18003=CARTESIAN_POINT('Ctrl Pts',(118.656113089351,-121.740461190303,-85.5433062032005));
#18004=CARTESIAN_POINT('Ctrl Pts',(118.73510902298,-121.663408950085,-85.4387098917068));
#18005=CARTESIAN_POINT('Ctrl Pts',(118.810850743183,-121.589398131891,-85.3292725022762));
#18006=CARTESIAN_POINT('Ctrl Pts',(118.830778159304,-121.569926110822,-85.3004798581098));
#18007=CARTESIAN_POINT('Ctrl Pts',(118.850480457642,-121.55066448544,-85.2713523136894));
#18008=CARTESIAN_POINT('Ctrl Pts',(118.869952060987,-121.531619330202,-85.2418842081897));
#18009=CARTESIAN_POINT('Ctrl Pts',(118.873852582751,-121.527804233869,-85.2359812024218));
#18010=CARTESIAN_POINT('Ctrl Pts',(118.87774476105,-121.523996924348,-85.2300626384257));
#18011=CARTESIAN_POINT('Ctrl Pts',(118.881628379448,-121.520197619565,-85.2241287426541));
#18012=CARTESIAN_POINT('Ctrl Pts',(118.95393335679,-121.449462388123,-85.1136518225858));
#18013=CARTESIAN_POINT('Ctrl Pts',(119.02337219024,-121.381403002896,-84.997686167018));
#18014=CARTESIAN_POINT('Ctrl Pts',(119.088533293332,-121.317439625781,-84.8776565982198));
#18015=CARTESIAN_POINT('Ctrl Pts',(119.107675671506,-121.298649103585,-84.8423955101026));
#18016=CARTESIAN_POINT('Ctrl Pts',(119.126449081002,-121.280211875349,-84.806783878756));
#18017=CARTESIAN_POINT('Ctrl Pts',(119.144818331366,-121.262163368406,-84.7708581772728));
#18018=CARTESIAN_POINT('Ctrl Pts',(119.147770180269,-121.259263061406,-84.7650850923405));
#18019=CARTESIAN_POINT('Ctrl Pts',(119.150711776641,-121.256372617005,-84.7593040201353));
#18020=CARTESIAN_POINT('Ctrl Pts',(119.153643085904,-121.253492073365,-84.7535149461629));
#18021=CARTESIAN_POINT('Ctrl Pts',(119.21747721143,-121.190763453579,-84.6274482498757));
#18022=CARTESIAN_POINT('Ctrl Pts',(119.276475877687,-121.132687812744,-84.4974947071808));
#18023=CARTESIAN_POINT('Ctrl Pts',(119.3302916925,-121.079649407404,-84.3634783755698));
#18024=CARTESIAN_POINT('Ctrl Pts',(119.344664771979,-121.065483957748,-84.3276854141062));
#18025=CARTESIAN_POINT('Ctrl Pts',(119.358668331281,-121.05167764448,-84.2916027835657));
#18026=CARTESIAN_POINT('Ctrl Pts',(119.37229615525,-121.038237390605,-84.2552274353945));
#18027=CARTESIAN_POINT('Ctrl Pts',(119.374201887271,-121.036357888622,-84.2501406610181));
#18028=CARTESIAN_POINT('Ctrl Pts',(119.376100550482,-121.034485269244,-84.2450470253995));
#18029=CARTESIAN_POINT('Ctrl Pts',(119.377992089409,-121.032619589192,-84.2399466200188));
#18030=CARTESIAN_POINT('Ctrl Pts',(119.432704267991,-120.978655370581,-84.0924189714974));
#18031=CARTESIAN_POINT('Ctrl Pts',(119.481511542453,-120.930442075976,-83.9390510932668));
#18032=CARTESIAN_POINT('Ctrl Pts',(119.523061427335,-120.889361770021,-83.7819751614011));
#18033=CARTESIAN_POINT('Ctrl Pts',(119.530667692994,-120.881841467105,-83.7532202979454));
#18034=CARTESIAN_POINT('Ctrl Pts',(119.538030846415,-120.874560108481,-83.7243411856429));
#18035=CARTESIAN_POINT('Ctrl Pts',(119.545142732111,-120.867526032261,-83.6953509136308));
#18036=CARTESIAN_POINT('Ctrl Pts',(119.546090881023,-120.866588256825,-83.6914859619103));
#18037=CARTESIAN_POINT('Ctrl Pts',(119.547034430282,-120.865655009876,-83.6876198631647));
#18038=CARTESIAN_POINT('Ctrl Pts',(119.547973377994,-120.864726293782,-83.6837526181087));
#18039=CARTESIAN_POINT('Ctrl Pts',(119.593937460371,-120.819263077397,-83.4944402974946));
#18040=CARTESIAN_POINT('Ctrl Pts',(119.62890424618,-120.784628102355,-83.3022686788512));
#18041=CARTESIAN_POINT('Ctrl Pts',(119.65264519197,-120.761105073466,-83.1071682749086));
#18042=CARTESIAN_POINT('Ctrl Pts',(119.676892336666,-120.737080492046,-82.9079079856867));
#18043=CARTESIAN_POINT('Ctrl Pts',(119.689439200918,-120.724637683323,-82.7055895150371));
#18044=CARTESIAN_POINT('Ctrl Pts',(119.689439203101,-120.724637681159,-82.5));
#18045=CARTESIAN_POINT('',(102.653719754201,-135.507246376812,-87.5));
#18046=CARTESIAN_POINT('Origin',(0.,0.,-87.5));
#18047=CARTESIAN_POINT('',(95.8022538025509,-140.434782608696,-82.5));
#18048=CARTESIAN_POINT('Ctrl Pts',(102.653719754201,-135.507246376812,-87.5));
#18049=CARTESIAN_POINT('Ctrl Pts',(102.215883490062,-135.838929901929,-87.4999999991685));
#18050=CARTESIAN_POINT('Ctrl Pts',(101.781087350657,-136.164971110003,-87.4669218367414));
#18051=CARTESIAN_POINT('Ctrl Pts',(101.349415497286,-136.485515662914,-87.4008783684644));
#18052=CARTESIAN_POINT('Ctrl Pts',(101.07973591123,-136.68577037414,-87.3596188444822));
#18053=CARTESIAN_POINT('Ctrl Pts',(100.811275778686,-136.88387961001,-87.3054922341186));
#18054=CARTESIAN_POINT('Ctrl Pts',(100.544056427545,-137.079877141377,-87.2385159157322));
#18055=CARTESIAN_POINT('Ctrl Pts',(100.541162556084,-137.081999710944,-87.2377905908054));
#18056=CARTESIAN_POINT('Ctrl Pts',(100.538268831608,-137.084122031661,-87.2370637322218));
#18057=CARTESIAN_POINT('Ctrl Pts',(100.535375254373,-137.086244103409,-87.2363353381554));
#18058=CARTESIAN_POINT('Ctrl Pts',(100.190565643195,-137.339118201716,-87.1495371453096));
#18059=CARTESIAN_POINT('Ctrl Pts',(99.8478512789412,-137.588453369916,-87.040933511602));
#18060=CARTESIAN_POINT('Ctrl Pts',(99.5077977395583,-137.833951510589,-86.9074976668159));
#18061=CARTESIAN_POINT('Ctrl Pts',(99.5037755731161,-137.836855272111,-86.9059193824726));
#18062=CARTESIAN_POINT('Ctrl Pts',(99.4997536170413,-137.839758608548,-86.9043375053786));
#18063=CARTESIAN_POINT('Ctrl Pts',(99.4957318889749,-137.842661507683,-86.9027520347699));
#18064=CARTESIAN_POINT('Ctrl Pts',(99.2674376143156,-138.007445213001,-86.8127524483652));
#18065=CARTESIAN_POINT('Ctrl Pts',(99.0398204570979,-138.170861151964,-86.711145683115));
#18066=CARTESIAN_POINT('Ctrl Pts',(98.8161737755042,-138.33062666086,-86.597820472154));
#18067=CARTESIAN_POINT('Ctrl Pts',(98.7076262937751,-138.408169254089,-86.5428177948124));
#18068=CARTESIAN_POINT('Ctrl Pts',(98.600013904115,-138.484852125992,-86.4850552618045));
#18069=CARTESIAN_POINT('Ctrl Pts',(98.4937108917853,-138.56041611792,-86.4245237415767));
#18070=CARTESIAN_POINT('Ctrl Pts',(98.4889708281906,-138.563785525046,-86.4218246341001));
#18071=CARTESIAN_POINT('Ctrl Pts',(98.4842329483831,-138.56715301161,-86.419119965262));
#18072=CARTESIAN_POINT('Ctrl Pts',(98.479497264693,-138.570518570128,-86.4164097092555));
#18073=CARTESIAN_POINT('Ctrl Pts',(98.2490703748719,-138.73427849005,-86.2845352212039));
#18074=CARTESIAN_POINT('Ctrl Pts',(98.0238750005084,-138.8934512373,-86.1394754931963));
#18075=CARTESIAN_POINT('Ctrl Pts',(97.8050966305876,-139.047339894881,-85.9780962529129));
#18076=CARTESIAN_POINT('Ctrl Pts',(97.7156206980972,-139.110277246236,-85.9120954045925));
#18077=CARTESIAN_POINT('Ctrl Pts',(97.6272183327067,-139.172330541299,-85.8433644738521));
#18078=CARTESIAN_POINT('Ctrl Pts',(97.5399718160535,-139.233451074562,-85.7716868356771));
#18079=CARTESIAN_POINT('Ctrl Pts',(97.5352562713784,-139.236754548629,-85.7678127657659));
#18080=CARTESIAN_POINT('Ctrl Pts',(97.5305452293931,-139.240054504138,-85.7639310032341));
#18081=CARTESIAN_POINT('Ctrl Pts',(97.5258387376046,-139.243350910624,-85.7600415156019));
#18082=CARTESIAN_POINT('Ctrl Pts',(97.3552183240805,-139.362852710079,-85.6190392536152));
#18083=CARTESIAN_POINT('Ctrl Pts',(97.1907405919816,-139.47757645948,-85.4680354210839));
#18084=CARTESIAN_POINT('Ctrl Pts',(97.0346910654179,-139.586057153202,-85.3056163231383));
#18085=CARTESIAN_POINT('Ctrl Pts',(96.9159928871056,-139.668572371353,-85.1820731668481));
#18086=CARTESIAN_POINT('Ctrl Pts',(96.8021704778946,-139.747475893107,-85.0519259141839));
#18087=CARTESIAN_POINT('Ctrl Pts',(96.694215926304,-139.822132033515,-84.9145642707921));
#18088=CARTESIAN_POINT('Ctrl Pts',(96.6906380099125,-139.824606347239,-84.9100117209624));
#18089=CARTESIAN_POINT('Ctrl Pts',(96.6870657587802,-139.827076536154,-84.9054498746293));
#18090=CARTESIAN_POINT('Ctrl Pts',(96.6834992847061,-139.82954252561,-84.9008787661799));
#18091=CARTESIAN_POINT('Ctrl Pts',(96.5933790288425,-139.891854937294,-84.7853726796454));
#18092=CARTESIAN_POINT('Ctrl Pts',(96.5068951547278,-139.951522102754,-84.6638795752373));
#18093=CARTESIAN_POINT('Ctrl Pts',(96.4259038292281,-140.007303114121,-84.5370163776214));
#18094=CARTESIAN_POINT('Ctrl Pts',(96.3961160047755,-140.027818829404,-84.4903573232502));
#18095=CARTESIAN_POINT('Ctrl Pts',(96.3670708290736,-140.047809094726,-84.4429721152884));
#18096=CARTESIAN_POINT('Ctrl Pts',(96.3388592767016,-140.067213127358,-84.3948922769621));
#18097=CARTESIAN_POINT('Ctrl Pts',(96.3362565453866,-140.069003297665,-84.390456544423));
#18098=CARTESIAN_POINT('Ctrl Pts',(96.3336613068006,-140.070788207782,-84.3860158118469));
#18099=CARTESIAN_POINT('Ctrl Pts',(96.3310735989047,-140.072567833443,-84.3815700581723));
#18100=CARTESIAN_POINT('Ctrl Pts',(96.2565223686416,-140.123838412584,-84.2534889844106));
#18101=CARTESIAN_POINT('Ctrl Pts',(96.18818677241,-140.170746863762,-84.1211671345774));
#18102=CARTESIAN_POINT('Ctrl Pts',(96.126962800212,-140.212720695597,-83.9840977199587));
#18103=CARTESIAN_POINT('Ctrl Pts',(96.1019843048262,-140.229845412064,-83.9281753807562));
#18104=CARTESIAN_POINT('Ctrl Pts',(96.0781891189942,-140.246149048065,-83.8714630194104));
#18105=CARTESIAN_POINT('Ctrl Pts',(96.0556361395659,-140.261594051371,-83.8139272219729));
#18106=CARTESIAN_POINT('Ctrl Pts',(96.0542034790336,-140.262575183231,-83.8102723050498));
#18107=CARTESIAN_POINT('Ctrl Pts',(96.0527757857576,-140.263552881361,-83.8066133446794));
#18108=CARTESIAN_POINT('Ctrl Pts',(96.0513530943973,-140.264527122689,-83.802950400001));
#18109=CARTESIAN_POINT('Ctrl Pts',(95.9866237488953,-140.308852972491,-83.6362944279056));
#18110=CARTESIAN_POINT('Ctrl Pts',(95.9322125151014,-140.346047836819,-83.4612414093815));
#18111=CARTESIAN_POINT('Ctrl Pts',(95.8913844101215,-140.373937837985,-83.2831693720156));
#18112=CARTESIAN_POINT('Ctrl Pts',(95.883045620544,-140.379634131044,-83.2467996886822));
#18113=CARTESIAN_POINT('Ctrl Pts',(95.8752733682718,-140.384942326837,-83.2103039208797));
#18114=CARTESIAN_POINT('Ctrl Pts',(95.8680953540231,-140.38984398165,-83.1737276630787));
#18115=CARTESIAN_POINT('Ctrl Pts',(95.8676809810245,-140.390126944783,-83.1716161858517));
#18116=CARTESIAN_POINT('Ctrl Pts',(95.8672684958815,-140.390408616667,-83.1695042863138));
#18117=CARTESIAN_POINT('Ctrl Pts',(95.8668579005401,-140.390688996011,-83.1673919642828));
#18118=CARTESIAN_POINT('Ctrl Pts',(95.8468264218082,-140.404367701805,-83.0643393244232));
#18119=CARTESIAN_POINT('Ctrl Pts',(95.8312774654238,-140.414980545424,-82.9601876791363));
#18120=CARTESIAN_POINT('Ctrl Pts',(95.8204649814164,-140.422358778653,-82.855032721006));
#18121=CARTESIAN_POINT('Ctrl Pts',(95.8099639220234,-140.429524501655,-82.7529064695304));
#18122=CARTESIAN_POINT('Ctrl Pts',(95.8039305392802,-140.433639185389,-82.649833883227));
#18123=CARTESIAN_POINT('Ctrl Pts',(95.8025570944415,-140.434575788992,-82.5459117712175));
#18124=CARTESIAN_POINT('Ctrl Pts',(95.802355077537,-140.434713551904,-82.5306261020837));
#18125=CARTESIAN_POINT('Ctrl Pts',(95.8022538025544,-140.434782608693,-82.5153220699784));
#18126=CARTESIAN_POINT('Ctrl Pts',(95.8022538025544,-140.434782608693,-82.5));
#18127=CARTESIAN_POINT('',(95.8022538025509,-140.434782608696,82.5));
#18128=CARTESIAN_POINT('',(95.802253802551,-140.434782608696,115.));
#18129=CARTESIAN_POINT('',(102.653719754201,-135.507246376812,87.5));
#18130=CARTESIAN_POINT('Ctrl Pts',(95.8022538025509,-140.434782608696,82.5));
#18131=CARTESIAN_POINT('Ctrl Pts',(95.8022538066581,-140.434782605894,82.7267635628216));
#18132=CARTESIAN_POINT('Ctrl Pts',(95.82442316008,-140.419665963906,82.9488530674831));
#18133=CARTESIAN_POINT('Ctrl Pts',(95.8667225776694,-140.39078140277,83.1666939397165));
#18134=CARTESIAN_POINT('Ctrl Pts',(95.8671957348732,-140.390458302857,83.1691306866946));
#18135=CARTESIAN_POINT('Ctrl Pts',(95.8676714126208,-140.390133479021,83.1715669081132));
#18136=CARTESIAN_POINT('Ctrl Pts',(95.8681496080969,-140.389806933124,83.1740026044675));
#18137=CARTESIAN_POINT('Ctrl Pts',(95.9022176054037,-140.366542880454,83.3475284970882));
#18138=CARTESIAN_POINT('Ctrl Pts',(95.9496913058969,-140.334107437353,83.5193033103427));
#18139=CARTESIAN_POINT('Ctrl Pts',(96.0075075764076,-140.294541978645,83.6842311536385));
#18140=CARTESIAN_POINT('Ctrl Pts',(96.0214298424345,-140.28501454222,83.7239460866381));
#18141=CARTESIAN_POINT('Ctrl Pts',(96.0359516723965,-140.275073772703,83.7632638427573));
#18142=CARTESIAN_POINT('Ctrl Pts',(96.0510300136253,-140.264748363786,83.8021130045776));
#18143=CARTESIAN_POINT('Ctrl Pts',(96.0526816582041,-140.263617343775,83.8063684466409));
#18144=CARTESIAN_POINT('Ctrl Pts',(96.0543400150297,-140.262481684736,83.8106183997866));
#18145=CARTESIAN_POINT('Ctrl Pts',(96.0560050279566,-140.261341424076,83.8148627669174));
#18146=CARTESIAN_POINT('Ctrl Pts',(96.1087379306462,-140.22522803811,83.9492868276993));
#18147=CARTESIAN_POINT('Ctrl Pts',(96.1682453864418,-140.18443183692,84.0791983701197));
#18148=CARTESIAN_POINT('Ctrl Pts',(96.233756492817,-140.139445304686,84.2050184596988));
#18149=CARTESIAN_POINT('Ctrl Pts',(96.2645815930226,-140.118277682267,84.2642208924426));
#18150=CARTESIAN_POINT('Ctrl Pts',(96.2967352970668,-140.096182731474,84.322517794146));
#18151=CARTESIAN_POINT('Ctrl Pts',(96.3301343379528,-140.073213779952,84.379954552556));
#18152=CARTESIAN_POINT('Ctrl Pts',(96.333181322976,-140.071118329022,84.3851944917284));
#18153=CARTESIAN_POINT('Ctrl Pts',(96.3362387534725,-140.069015548404,84.3904274269311));
#18154=CARTESIAN_POINT('Ctrl Pts',(96.339306565948,-140.066905478751,84.395653391359));
#18155=CARTESIAN_POINT('Ctrl Pts',(96.4117861971904,-140.017053321377,84.5191211644543));
#18156=CARTESIAN_POINT('Ctrl Pts',(96.489984201705,-139.963182743649,84.6383213999031));
#18157=CARTESIAN_POINT('Ctrl Pts',(96.5721307821755,-139.906480636874,84.7523713006202));
#18158=CARTESIAN_POINT('Ctrl Pts',(96.6081754745549,-139.881600599455,84.8024146933422));
#18159=CARTESIAN_POINT('Ctrl Pts',(96.6449798263787,-139.856175797165,84.8514667731971));
#18160=CARTESIAN_POINT('Ctrl Pts',(96.6823922460869,-139.830307960496,84.8994546030534));
#18161=CARTESIAN_POINT('Ctrl Pts',(96.6866911658705,-139.827335585127,84.9049687032572));
#18162=CARTESIAN_POINT('Ctrl Pts',(96.6909982721174,-139.824357251048,84.910468962333));
#18163=CARTESIAN_POINT('Ctrl Pts',(96.6953133447454,-139.821373105703,84.9159552790206));
#18164=CARTESIAN_POINT('Ctrl Pts',(96.8598715711489,-139.707570695464,85.1251796933976));
#18165=CARTESIAN_POINT('Ctrl Pts',(97.0374177648447,-139.584350177983,85.3170893285477));
#18166=CARTESIAN_POINT('Ctrl Pts',(97.2253643458243,-139.453317347345,85.4947229628092));
#18167=CARTESIAN_POINT('Ctrl Pts',(97.3220405832959,-139.385916488094,85.5860944116501));
#18168=CARTESIAN_POINT('Ctrl Pts',(97.4214682311097,-139.316448807693,85.6736891876995));
#18169=CARTESIAN_POINT('Ctrl Pts',(97.5232920470747,-139.245134572953,85.7579251167103));
#18170=CARTESIAN_POINT('Ctrl Pts',(97.5293253469238,-139.24090903733,85.7629162930178));
#18171=CARTESIAN_POINT('Ctrl Pts',(97.5353667088665,-139.236677264114,85.7678953452721));
#18172=CARTESIAN_POINT('Ctrl Pts',(97.5414160595531,-139.232439298912,85.7728623680769));
#18173=CARTESIAN_POINT('Ctrl Pts',(97.7162996211817,-139.10992194342,85.9164563972194));
#18174=CARTESIAN_POINT('Ctrl Pts',(97.8952913851829,-138.984032327629,86.0478104714154));
#18175=CARTESIAN_POINT('Ctrl Pts',(98.0778068948705,-138.855116179527,86.1688889205228));
#18176=CARTESIAN_POINT('Ctrl Pts',(98.208102146782,-138.763084756986,86.255325120134));
#18177=CARTESIAN_POINT('Ctrl Pts',(98.3401938135588,-138.669510449023,86.3365230930489));
#18178=CARTESIAN_POINT('Ctrl Pts',(98.4738752709946,-138.57451383921,86.4131838583196));
#18179=CARTESIAN_POINT('Ctrl Pts',(98.4804799835179,-138.569820403707,86.4169713867184));
#18180=CARTESIAN_POINT('Ctrl Pts',(98.4870884834125,-138.565123562489,86.4207477533717));
#18181=CARTESIAN_POINT('Ctrl Pts',(98.4937007396701,-138.560423334432,86.424513039284));
#18182=CARTESIAN_POINT('Ctrl Pts',(98.7840182406829,-138.354055279349,86.589831556));
#18183=CARTESIAN_POINT('Ctrl Pts',(99.0816753157249,-138.141093442614,86.7335191053828));
#18184=CARTESIAN_POINT('Ctrl Pts',(99.3855316242237,-137.922137706692,86.8583876044078));
#18185=CARTESIAN_POINT('Ctrl Pts',(99.4178327967954,-137.898861813403,86.8716616382947));
#18186=CARTESIAN_POINT('Ctrl Pts',(99.4502040185954,-137.875518189568,86.8847230539631));
#18187=CARTESIAN_POINT('Ctrl Pts',(99.4826439161487,-137.852107558311,86.8975752625191));
#18188=CARTESIAN_POINT('Ctrl Pts',(99.4892006235699,-137.847375833759,86.9001729332139));
#18189=CARTESIAN_POINT('Ctrl Pts',(99.4957601913217,-137.842641332283,86.9027620700699));
#18190=CARTESIAN_POINT('Ctrl Pts',(99.5023226100944,-137.83790405835,86.9053427012608));
#18191=CARTESIAN_POINT('Ctrl Pts',(99.7610782414197,-137.651113737626,87.0070967764188));
#18192=CARTESIAN_POINT('Ctrl Pts',(100.023540548063,-137.460524429705,87.0951230469053));
#18193=CARTESIAN_POINT('Ctrl Pts',(100.286778082508,-137.268209583308,87.1698025078672));
#18194=CARTESIAN_POINT('Ctrl Pts',(100.367689287584,-137.209097853635,87.1927567009067));
#18195=CARTESIAN_POINT('Ctrl Pts',(100.448673514288,-137.149823232307,87.2144496896512));
#18196=CARTESIAN_POINT('Ctrl Pts',(100.529644945652,-137.09044635394,87.2348918842082));
#18197=CARTESIAN_POINT('Ctrl Pts',(100.535236887059,-137.086345746859,87.2363036358874));
#18198=CARTESIAN_POINT('Ctrl Pts',(100.54082877009,-137.082244650117,87.2377094234242));
#18199=CARTESIAN_POINT('Ctrl Pts',(100.546420565381,-137.078143084482,87.2391092498982));
#18200=CARTESIAN_POINT('Ctrl Pts',(101.006759430624,-136.740485861341,87.3543485419369));
#18201=CARTESIAN_POINT('Ctrl Pts',(101.469785371656,-136.397290219446,87.4312211195578));
#18202=CARTESIAN_POINT('Ctrl Pts',(101.935255321594,-136.048534052163,87.4701010401868));
#18203=CARTESIAN_POINT('Ctrl Pts',(102.174111254841,-135.869569803615,87.4900522738327));
#18204=CARTESIAN_POINT('Ctrl Pts',(102.41361062282,-135.689141412998,87.4999999996522));
#18205=CARTESIAN_POINT('Ctrl Pts',(102.653719754201,-135.507246376812,87.5));
#18206=CARTESIAN_POINT('',(114.505594583524,-125.652173913043,87.5));
#18207=CARTESIAN_POINT('Origin',(0.,0.,87.5));
#18208=CARTESIAN_POINT('Ctrl Pts',(119.689439203101,-120.724637681159,82.5));
#18209=CARTESIAN_POINT('Ctrl Pts',(119.689439202149,-120.724637682103,82.7035326184388));
#18210=CARTESIAN_POINT('Ctrl Pts',(119.677137855384,-120.736837058147,82.9047280297056));
#18211=CARTESIAN_POINT('Ctrl Pts',(119.653068783703,-120.760685368386,83.1036884565072));
#18212=CARTESIAN_POINT('Ctrl Pts',(119.653066214653,-120.760687913874,83.1037096928656));
#18213=CARTESIAN_POINT('Ctrl Pts',(119.653063645461,-120.7606904595,83.1037309292184));
#18214=CARTESIAN_POINT('Ctrl Pts',(119.65306107613,-120.760693005265,83.1037521655658));
#18215=CARTESIAN_POINT('Ctrl Pts',(119.641919852112,-120.771732040823,83.1958379462712));
#18216=CARTESIAN_POINT('Ctrl Pts',(119.628149514819,-120.785373482771,83.2877525623368));
#18217=CARTESIAN_POINT('Ctrl Pts',(119.611957511351,-120.801406080558,83.3788351082885));
#18218=CARTESIAN_POINT('Ctrl Pts',(119.594967539022,-120.818228791431,83.4744063535959));
#18219=CARTESIAN_POINT('Ctrl Pts',(119.575311134738,-120.837684355099,83.5690634426131));
#18220=CARTESIAN_POINT('Ctrl Pts',(119.553189137451,-120.859567147649,83.6620443511901));
#18221=CARTESIAN_POINT('Ctrl Pts',(119.550837400782,-120.861893455034,83.6719289293931));
#18222=CARTESIAN_POINT('Ctrl Pts',(119.548457766993,-120.864247225519,83.6817945489539));
#18223=CARTESIAN_POINT('Ctrl Pts',(119.546050454752,-120.866628234349,83.6916402803607));
#18224=CARTESIAN_POINT('Ctrl Pts',(119.545706019787,-120.866968905857,83.6930489942347));
#18225=CARTESIAN_POINT('Ctrl Pts',(119.545361019709,-120.867310133486,83.6944572963286));
#18226=CARTESIAN_POINT('Ctrl Pts',(119.545015455303,-120.867651916433,83.6958651833482));
#18227=CARTESIAN_POINT('Ctrl Pts',(119.498574793915,-120.913584384682,83.8850721826734));
#18228=CARTESIAN_POINT('Ctrl Pts',(119.442053836954,-120.969435426432,84.0677448259361));
#18229=CARTESIAN_POINT('Ctrl Pts',(119.376325844471,-121.034263033589,84.2444400249401));
#18230=CARTESIAN_POINT('Ctrl Pts',(119.375341514618,-121.035233879443,84.2470861784681));
#18231=CARTESIAN_POINT('Ctrl Pts',(119.374355124207,-121.036206734213,84.2497309822512));
#18232=CARTESIAN_POINT('Ctrl Pts',(119.373366676024,-121.037181594879,84.2523744389027));
#18233=CARTESIAN_POINT('Ctrl Pts',(119.316775771354,-121.09299458329,84.4037183393109));
#18234=CARTESIAN_POINT('Ctrl Pts',(119.253023740074,-121.155791267856,84.5514088442846));
#18235=CARTESIAN_POINT('Ctrl Pts',(119.183533814645,-121.224111670241,84.6934551431387));
#18236=CARTESIAN_POINT('Ctrl Pts',(119.172587065774,-121.234874184132,84.7158316984741));
#18237=CARTESIAN_POINT('Ctrl Pts',(119.161497891706,-121.24577380549,84.7380680951027));
#18238=CARTESIAN_POINT('Ctrl Pts',(119.150271823512,-121.256804856299,84.7601564357349));
#18239=CARTESIAN_POINT('Ctrl Pts',(119.148539861699,-121.258506730759,84.7635642328208));
#18240=CARTESIAN_POINT('Ctrl Pts',(119.146804666256,-121.260211709207,84.7669684593409));
#18241=CARTESIAN_POINT('Ctrl Pts',(119.14506625839,-121.261919769913,84.7703690853657));
#18242=CARTESIAN_POINT('Ctrl Pts',(119.003325684158,-121.401185997451,85.0476381285352));
#18243=CARTESIAN_POINT('Ctrl Pts',(118.842142582395,-121.559065373447,85.2991641768823));
#18244=CARTESIAN_POINT('Ctrl Pts',(118.664609105015,-121.732125921824,85.5295568165563));
#18245=CARTESIAN_POINT('Ctrl Pts',(118.63378202579,-121.76217631747,85.5695624102107));
#18246=CARTESIAN_POINT('Ctrl Pts',(118.602462004168,-121.79268438568,85.6089309118895));
#18247=CARTESIAN_POINT('Ctrl Pts',(118.570665287738,-121.823632077489,85.6476865935974));
#18248=CARTESIAN_POINT('Ctrl Pts',(118.567733597815,-121.826485486471,85.6512599072698));
#18249=CARTESIAN_POINT('Ctrl Pts',(118.564797840986,-121.829342646821,85.6548280160811));
#18250=CARTESIAN_POINT('Ctrl Pts',(118.561858031783,-121.832203542636,85.6583909367604));
#18251=CARTESIAN_POINT('Ctrl Pts',(118.462775019687,-121.928626866429,85.7784752308077));
#18252=CARTESIAN_POINT('Ctrl Pts',(118.358568310361,-122.029796769546,85.8929376116578));
#18253=CARTESIAN_POINT('Ctrl Pts',(118.251586147631,-122.133379333937,86.0001705914024));
#18254=CARTESIAN_POINT('Ctrl Pts',(118.244181404727,-122.140548774516,86.0075926945414));
#18255=CARTESIAN_POINT('Ctrl Pts',(118.236763378118,-122.147729761558,86.0149801740683));
#18256=CARTESIAN_POINT('Ctrl Pts',(118.229332851436,-122.154921516527,86.0223325018977));
#18257=CARTESIAN_POINT('Ctrl Pts',(118.226055490992,-122.158093562638,86.0255753714058));
#18258=CARTESIAN_POINT('Ctrl Pts',(118.222775639178,-122.161267761231,86.0288114700421));
#18259=CARTESIAN_POINT('Ctrl Pts',(118.219493362288,-122.164444046394,86.0320407520764));
#18260=CARTESIAN_POINT('Ctrl Pts',(118.104628229969,-122.27559993839,86.1450512994916));
#18261=CARTESIAN_POINT('Ctrl Pts',(117.986476048706,-122.389622505763,86.2501973510142));
#18262=CARTESIAN_POINT('Ctrl Pts',(117.865390836685,-122.506120837556,86.3482582753081));
#18263=CARTESIAN_POINT('Ctrl Pts',(117.861984025646,-122.509398593743,86.3510172830664));
#18264=CARTESIAN_POINT('Ctrl Pts',(117.858574879434,-122.512678322681,86.3537706967459));
#18265=CARTESIAN_POINT('Ctrl Pts',(117.855163404827,-122.515960016733,86.3565185352213));
#18266=CARTESIAN_POINT('Ctrl Pts',(117.634786727148,-122.727953044864,86.5340252101117));
#18267=CARTESIAN_POINT('Ctrl Pts',(117.404749933279,-122.948091220296,86.6884140414481));
#18268=CARTESIAN_POINT('Ctrl Pts',(117.165977820927,-123.175215090991,86.8223776639549));
#18269=CARTESIAN_POINT('Ctrl Pts',(117.138194024572,-123.201643484612,86.8379658244401));
#18270=CARTESIAN_POINT('Ctrl Pts',(117.11029196616,-123.228166449504,86.8532774834095));
#18271=CARTESIAN_POINT('Ctrl Pts',(117.082273113257,-123.25478214762,86.8683169246699));
#18272=CARTESIAN_POINT('Ctrl Pts',(117.07907454041,-123.257820539291,86.8700337954002));
#18273=CARTESIAN_POINT('Ctrl Pts',(117.075874453948,-123.260860131433,86.871747111702));
#18274=CARTESIAN_POINT('Ctrl Pts',(117.072672856275,-123.263900921107,86.8734568798933));
#18275=CARTESIAN_POINT('Ctrl Pts',(116.860769276682,-123.465161130014,86.9866210051082));
#18276=CARTESIAN_POINT('Ctrl Pts',(116.644679573649,-123.669347678144,87.082787673174));
#18277=CARTESIAN_POINT('Ctrl Pts',(116.426318407412,-123.874581811768,87.1633254409075));
#18278=CARTESIAN_POINT('Ctrl Pts',(116.366869225742,-123.930457137519,87.1852519787982));
#18279=CARTESIAN_POINT('Ctrl Pts',(116.307251761957,-123.986410050552,87.2060203754224));
#18280=CARTESIAN_POINT('Ctrl Pts',(116.247504799008,-124.042402536954,87.2256588635444));
#18281=CARTESIAN_POINT('Ctrl Pts',(116.245124621172,-124.044633145315,87.2264412145101));
#18282=CARTESIAN_POINT('Ctrl Pts',(116.242744233986,-124.046863820072,87.2272217734333));
#18283=CARTESIAN_POINT('Ctrl Pts',(116.24036363979,-124.049094558926,87.2280005421223));
#18284=CARTESIAN_POINT('Ctrl Pts',(115.8311772319,-124.432523208838,87.3618585356373));
#18285=CARTESIAN_POINT('Ctrl Pts',(115.413668084723,-124.819944300696,87.4448575139198));
#18286=CARTESIAN_POINT('Ctrl Pts',(114.988112172538,-125.210757502246,87.4801920397485));
#18287=CARTESIAN_POINT('Ctrl Pts',(114.828401703243,-125.357429086495,87.4934530321137));
#18288=CARTESIAN_POINT('Ctrl Pts',(114.667557757302,-125.504578460163,87.4999999998164));
#18289=CARTESIAN_POINT('Ctrl Pts',(114.505594583524,-125.652173913043,87.5));
#18290=CARTESIAN_POINT('',(145.36231884058,-88.1464478086873,49.5));
#18291=CARTESIAN_POINT('Origin',(0.,0.,49.5));
#18292=CARTESIAN_POINT('',(150.289855072464,-79.4541343310581,44.5));
#18293=CARTESIAN_POINT('Ctrl Pts',(145.36231884058,-88.1464478086873,49.5));
#18294=CARTESIAN_POINT('Ctrl Pts',(145.729245608051,-87.5413488274995,49.4999999993448));
#18295=CARTESIAN_POINT('Ctrl Pts',(146.089427497743,-86.938852139224,49.459451627546));
#18296=CARTESIAN_POINT('Ctrl Pts',(146.443059008834,-86.3390437438767,49.3785345234731));
#18297=CARTESIAN_POINT('Ctrl Pts',(146.591729818533,-86.0868773022461,49.3445160296351));
#18298=CARTESIAN_POINT('Ctrl Pts',(146.739242767663,-85.8351860376504,49.3033619016674));
#18299=CARTESIAN_POINT('Ctrl Pts',(146.885611849037,-85.5839764893769,49.2550827834563));
#18300=CARTESIAN_POINT('Ctrl Pts',(146.887215711036,-85.581223821639,49.2545537575016));
#18301=CARTESIAN_POINT('Ctrl Pts',(146.888819435246,-85.5784712124141,49.2540238618083));
#18302=CARTESIAN_POINT('Ctrl Pts',(146.890423021642,-85.5757186617924,49.2534930956204));
#18303=CARTESIAN_POINT('Ctrl Pts',(147.136163003217,-85.1539068149984,49.1721563659123));
#18304=CARTESIAN_POINT('Ctrl Pts',(147.378654044698,-84.733492627337,49.0703840441395));
#18305=CARTESIAN_POINT('Ctrl Pts',(147.617771548819,-84.3148475830954,48.9454703779811));
#18306=CARTESIAN_POINT('Ctrl Pts',(147.619992196193,-84.3109596911514,48.9443103240332));
#18307=CARTESIAN_POINT('Ctrl Pts',(147.622212556282,-84.307071941363,48.943148258573));
#18308=CARTESIAN_POINT('Ctrl Pts',(147.624432625828,-84.303184339794,48.9419841796181));
#18309=CARTESIAN_POINT('Ctrl Pts',(147.797445356911,-84.0002188016352,48.8512660849843));
#18310=CARTESIAN_POINT('Ctrl Pts',(147.968707326118,-83.6981287755317,48.7483109143164));
#18311=CARTESIAN_POINT('Ctrl Pts',(148.136615104019,-83.3998939012959,48.6322285684957));
#18312=CARTESIAN_POINT('Ctrl Pts',(148.200188500854,-83.2869759397415,48.5882773642776));
#18313=CARTESIAN_POINT('Ctrl Pts',(148.263281189795,-83.1746104678287,48.5424447848479));
#18314=CARTESIAN_POINT('Ctrl Pts',(148.325806750807,-83.0629583612551,48.4946842709289));
#18315=CARTESIAN_POINT('Ctrl Pts',(148.328437713,-83.0582602431345,48.4926745951353));
#18316=CARTESIAN_POINT('Ctrl Pts',(148.331067922545,-83.0535629380485,48.4906613522023));
#18317=CARTESIAN_POINT('Ctrl Pts',(148.333697371916,-83.0488664605796,48.4886445330394));
#18318=CARTESIAN_POINT('Ctrl Pts',(148.479392264376,-82.7886398186652,48.3768948053783));
#18319=CARTESIAN_POINT('Ctrl Pts',(148.622808981178,-82.5308543489962,48.2541267340886));
#18320=CARTESIAN_POINT('Ctrl Pts',(148.762663381336,-82.2779954776877,48.1187795814413));
#18321=CARTESIAN_POINT('Ctrl Pts',(148.840976563632,-82.1364040593145,48.0429902875284));
#18322=CARTESIAN_POINT('Ctrl Pts',(148.918172933796,-81.9963571587517,47.9632574413117));
#18323=CARTESIAN_POINT('Ctrl Pts',(148.994029023493,-81.8582880066048,47.8793133555439));
#18324=CARTESIAN_POINT('Ctrl Pts',(148.996712266487,-81.8534041128184,47.8763440174079));
#18325=CARTESIAN_POINT('Ctrl Pts',(148.999393672824,-81.8485229853453,47.8733697901463));
#18326=CARTESIAN_POINT('Ctrl Pts',(149.002073232327,-81.8436446453373,47.8703906395336));
#18327=CARTESIAN_POINT('Ctrl Pts',(149.107681065302,-81.6513776267181,47.7529752061311));
#18328=CARTESIAN_POINT('Ctrl Pts',(149.210443318177,-81.4633981454557,47.6279048759376));
#18329=CARTESIAN_POINT('Ctrl Pts',(149.309720948425,-81.2810297213993,47.4931045485117));
#18330=CARTESIAN_POINT('Ctrl Pts',(149.401996350024,-81.111524068145,47.3678119290385));
#18331=CARTESIAN_POINT('Ctrl Pts',(149.491261252891,-80.9468661107977,47.2341131033335));
#18332=CARTESIAN_POINT('Ctrl Pts',(149.577013895448,-80.7880986852943,47.0903818425147));
#18333=CARTESIAN_POINT('Ctrl Pts',(149.583521150904,-80.7760507744081,47.0794749362875));
#18334=CARTESIAN_POINT('Ctrl Pts',(149.590008187584,-80.7640367723622,47.0685102812695));
#18335=CARTESIAN_POINT('Ctrl Pts',(149.596474789369,-80.752057129177,47.0574871779499));
#18336=CARTESIAN_POINT('Ctrl Pts',(149.598641974416,-80.7480423306098,47.0537929494384));
#18337=CARTESIAN_POINT('Ctrl Pts',(149.600807137209,-80.7440308818109,47.050091283938));
#18338=CARTESIAN_POINT('Ctrl Pts',(149.602970226706,-80.7400228807506,47.0463821931637));
#18339=CARTESIAN_POINT('Ctrl Pts',(149.665071318886,-80.6249554072859,46.9398962671819));
#18340=CARTESIAN_POINT('Ctrl Pts',(149.72550325001,-80.5126559819617,46.8272204519951));
#18341=CARTESIAN_POINT('Ctrl Pts',(149.783030801752,-80.4054929778246,46.7086718150296));
#18342=CARTESIAN_POINT('Ctrl Pts',(149.809543928151,-80.3561040122254,46.6540354729443));
#18343=CARTESIAN_POINT('Ctrl Pts',(149.835440369712,-80.3078056559303,46.5981521261349));
#18344=CARTESIAN_POINT('Ctrl Pts',(149.860600799428,-80.260826858675,46.5410549251661));
#18345=CARTESIAN_POINT('Ctrl Pts',(149.862244464557,-80.2577578566065,46.5373249142225));
#18346=CARTESIAN_POINT('Ctrl Pts',(149.863885113163,-80.2546942576169,46.5335897131967));
#18347=CARTESIAN_POINT('Ctrl Pts',(149.865522721631,-80.2516361085815,46.5298492852785));
#18348=CARTESIAN_POINT('Ctrl Pts',(149.920874283176,-80.148269932952,46.4034219187085));
#18349=CARTESIAN_POINT('Ctrl Pts',(149.972772946679,-80.0510921736928,46.2709925001795));
#18350=CARTESIAN_POINT('Ctrl Pts',(150.020328326584,-79.961871940831,46.1310781770696));
#18351=CARTESIAN_POINT('Ctrl Pts',(150.041423437799,-79.9222946997582,46.0690135229251));
#18352=CARTESIAN_POINT('Ctrl Pts',(150.061664115444,-79.884282891071,46.0054765146034));
#18353=CARTESIAN_POINT('Ctrl Pts',(150.080973718749,-79.8479888765764,45.9403401621094));
#18354=CARTESIAN_POINT('Ctrl Pts',(150.081910893431,-79.8462273783758,45.9371788262994));
#18355=CARTESIAN_POINT('Ctrl Pts',(150.082845417364,-79.8444707888363,45.9340152250091));
#18356=CARTESIAN_POINT('Ctrl Pts',(150.083777280819,-79.842719127427,45.9308493494822));
#18357=CARTESIAN_POINT('Ctrl Pts',(150.124316972743,-79.7665150295208,45.7931214259646));
#18358=CARTESIAN_POINT('Ctrl Pts',(150.159836015379,-79.6996105779127,45.6510364734858));
#18359=CARTESIAN_POINT('Ctrl Pts',(150.189536570941,-79.643601630539,45.5038983003528));
#18360=CARTESIAN_POINT('Ctrl Pts',(150.205994764956,-79.6125649679259,45.4223635090175));
#18361=CARTESIAN_POINT('Ctrl Pts',(150.22066665991,-79.5848732537911,45.3392772231722));
#18362=CARTESIAN_POINT('Ctrl Pts',(150.233419649245,-79.5607919801431,45.2545226584932));
#18363=CARTESIAN_POINT('Ctrl Pts',(150.233653158554,-79.5603510481059,45.252970788629));
#18364=CARTESIAN_POINT('Ctrl Pts',(150.233885994755,-79.5599113833124,45.2514181977489));
#18365=CARTESIAN_POINT('Ctrl Pts',(150.234118156878,-79.5594729876405,45.2498648923104));
#18366=CARTESIAN_POINT('Ctrl Pts',(150.243593980634,-79.5415796290569,45.1864658831964));
#18367=CARTESIAN_POINT('Ctrl Pts',(150.251930637624,-79.5258311439937,45.1219886580334));
#18368=CARTESIAN_POINT('Ctrl Pts',(150.25908694937,-79.5123085902624,45.0567119030525));
#18369=CARTESIAN_POINT('Ctrl Pts',(150.266133192886,-79.4989940212598,44.9924391424681));
#18370=CARTESIAN_POINT('Ctrl Pts',(150.272035277524,-79.4878371314994,44.9273898861929));
#18371=CARTESIAN_POINT('Ctrl Pts',(150.276731655023,-79.4789572453975,44.8618164804335));
#18372=CARTESIAN_POINT('Ctrl Pts',(150.281154338818,-79.4705948579246,44.8000645367055));
#18373=CARTESIAN_POINT('Ctrl Pts',(150.284507727575,-79.4642518495708,44.7378467346804));
#18374=CARTESIAN_POINT('Ctrl Pts',(150.286719886614,-79.4600667280322,44.6753785307951));
#18375=CARTESIAN_POINT('Ctrl Pts',(150.28878458935,-79.4561605749315,44.6170742817893));
#18376=CARTESIAN_POINT('Ctrl Pts',(150.289855072332,-79.4541343313065,44.5585512837797));
#18377=CARTESIAN_POINT('Ctrl Pts',(150.289855072464,-79.4541343310581,44.5));
#18378=CARTESIAN_POINT('',(150.289855072464,-79.4541343310581,37.5));
#18379=CARTESIAN_POINT('',(150.289855072464,-79.4541343310581,115.));
#18380=CARTESIAN_POINT('',(145.36231884058,-88.1464478086873,32.5));
#18381=CARTESIAN_POINT('Ctrl Pts',(150.289855072464,-79.4541343310581,37.5));
#18382=CARTESIAN_POINT('Ctrl Pts',(150.289855068577,-79.4541343384106,37.2436476198539));
#18383=CARTESIAN_POINT('Ctrl Pts',(150.270581238553,-79.4906188049207,36.9946184779966));
#18384=CARTESIAN_POINT('Ctrl Pts',(150.23440031069,-79.5589401936918,36.7519883573953));
#18385=CARTESIAN_POINT('Ctrl Pts',(150.233993766309,-79.5597078820386,36.7492620615822));
#18386=CARTESIAN_POINT('Ctrl Pts',(150.2335850823,-79.5604795994257,36.7465365450198));
#18387=CARTESIAN_POINT('Ctrl Pts',(150.233174261933,-79.5612553394204,36.7438118068128));
#18388=CARTESIAN_POINT('Ctrl Pts',(150.211108362005,-79.6029217280991,36.597461222919));
#18389=CARTESIAN_POINT('Ctrl Pts',(150.183223768723,-79.6555340186059,36.4560333910476));
#18390=CARTESIAN_POINT('Ctrl Pts',(150.150657295397,-79.7168744981781,36.3199679218119));
#18391=CARTESIAN_POINT('Ctrl Pts',(150.129869982028,-79.7560283776372,36.2331167752582));
#18392=CARTESIAN_POINT('Ctrl Pts',(150.107175698373,-79.7987372958168,36.1484502336036));
#18393=CARTESIAN_POINT('Ctrl Pts',(150.082875014061,-79.8444151271613,36.0660801928035));
#18394=CARTESIAN_POINT('Ctrl Pts',(150.081600916097,-79.8468100404567,36.0617614872072));
#18395=CARTESIAN_POINT('Ctrl Pts',(150.080322360848,-79.8492131928944,36.0574489500033));
#18396=CARTESIAN_POINT('Ctrl Pts',(150.079039391808,-79.8516244996445,36.05314260126));
#18397=CARTESIAN_POINT('Ctrl Pts',(150.044542112121,-79.9164612343937,35.9373507837354));
#18398=CARTESIAN_POINT('Ctrl Pts',(150.006537123162,-79.9877842271916,35.8251345490234));
#18399=CARTESIAN_POINT('Ctrl Pts',(149.965970804577,-80.0637685565931,35.717265369449));
#18400=CARTESIAN_POINT('Ctrl Pts',(149.933351576219,-80.124867277869,35.6305281568029));
#18401=CARTESIAN_POINT('Ctrl Pts',(149.899077126142,-80.1889782570248,35.5466015578877));
#18402=CARTESIAN_POINT('Ctrl Pts',(149.863649966461,-80.255133246411,35.4658772780751));
#18403=CARTESIAN_POINT('Ctrl Pts',(149.861515024356,-80.2591199355374,35.4610126017817));
#18404=CARTESIAN_POINT('Ctrl Pts',(149.85937578758,-80.2631142503699,35.4561592869362));
#18405=CARTESIAN_POINT('Ctrl Pts',(149.857232364154,-80.2671159825673,35.4513174183972));
#18406=CARTESIAN_POINT('Ctrl Pts',(149.804252858278,-80.3660277477068,35.331639803768));
#18407=CARTESIAN_POINT('Ctrl Pts',(149.748484158478,-80.4699094430571,35.2180933719206));
#18408=CARTESIAN_POINT('Ctrl Pts',(149.690355247896,-80.5778965450401,35.1097499748562));
#18409=CARTESIAN_POINT('Ctrl Pts',(149.661473306407,-80.6315510369237,35.0559184541312));
#18410=CARTESIAN_POINT('Ctrl Pts',(149.63200898673,-80.6862185045824,35.0033707288664));
#18411=CARTESIAN_POINT('Ctrl Pts',(149.60201639041,-80.741790230842,34.9519894923051));
#18412=CARTESIAN_POINT('Ctrl Pts',(149.599223408299,-80.7469652025476,34.9472047489959));
#18413=CARTESIAN_POINT('Ctrl Pts',(149.596425806469,-80.7521480873936,34.9424300694399));
#18414=CARTESIAN_POINT('Ctrl Pts',(149.593623625112,-80.7573388040449,34.9376653528747));
#18415=CARTESIAN_POINT('Ctrl Pts',(149.503321107799,-80.9246137661054,34.7841185815494));
#18416=CARTESIAN_POINT('Ctrl Pts',(149.407759531995,-81.1009468141059,34.6404004213219));
#18417=CARTESIAN_POINT('Ctrl Pts',(149.309404815745,-81.2816192446479,34.5068550549142));
#18418=CARTESIAN_POINT('Ctrl Pts',(149.306147321137,-81.2876030905749,34.5024320508374));
#18419=CARTESIAN_POINT('Ctrl Pts',(149.302886794892,-81.2935916372183,34.498020248125));
#18420=CARTESIAN_POINT('Ctrl Pts',(149.299623326396,-81.2995847135534,34.4936196571957));
#18421=CARTESIAN_POINT('Ctrl Pts',(149.201294060241,-81.4801578671638,34.3610285574972));
#18422=CARTESIAN_POINT('Ctrl Pts',(149.100390942177,-81.6646756184357,34.2385852650971));
#18423=CARTESIAN_POINT('Ctrl Pts',(148.997297013874,-81.8523394986245,34.1242886774831));
#18424=CARTESIAN_POINT('Ctrl Pts',(148.993783486671,-81.8587352404397,34.1203933542914));
#18425=CARTESIAN_POINT('Ctrl Pts',(148.99026742009,-81.8651346268365,34.1165075135218));
#18426=CARTESIAN_POINT('Ctrl Pts',(148.986748829868,-81.871537625153,34.1126310765379));
#18427=CARTESIAN_POINT('Ctrl Pts',(148.82898957284,-82.158621995175,33.9388274279259));
#18428=CARTESIAN_POINT('Ctrl Pts',(148.666197518725,-82.4528887104821,33.7837344929974));
#18429=CARTESIAN_POINT('Ctrl Pts',(148.499047675039,-82.7528397905726,33.6438439855164));
#18430=CARTESIAN_POINT('Ctrl Pts',(148.443888606591,-82.8518229651463,33.5976804360501));
#18431=CARTESIAN_POINT('Ctrl Pts',(148.388255039764,-82.95142505779,33.5531719899696));
#18432=CARTESIAN_POINT('Ctrl Pts',(148.332171389768,-83.0515919680528,33.5101914075088));
#18433=CARTESIAN_POINT('Ctrl Pts',(148.328463625565,-83.0582141348388,33.507349904413));
#18434=CARTESIAN_POINT('Ctrl Pts',(148.324753888106,-83.0648387811286,33.5045150857075));
#18435=CARTESIAN_POINT('Ctrl Pts',(148.321042184227,-83.0714658916725,33.5016869147104));
#18436=CARTESIAN_POINT('Ctrl Pts',(148.127526079484,-83.4169817679298,33.3542353256982));
#18437=CARTESIAN_POINT('Ctrl Pts',(147.928023779053,-83.7703038873448,33.224894934723));
#18438=CARTESIAN_POINT('Ctrl Pts',(147.726117191227,-84.1248695147591,33.1128740239443));
#18439=CARTESIAN_POINT('Ctrl Pts',(147.691851026841,-84.1850438964133,33.0938626237485));
#18440=CARTESIAN_POINT('Ctrl Pts',(147.657515670422,-84.2452539899407,33.0753500432994));
#18441=CARTESIAN_POINT('Ctrl Pts',(147.623128700903,-84.3054675885421,33.0573323830867));
#18442=CARTESIAN_POINT('Ctrl Pts',(147.61966084937,-84.3115399997818,33.0555153410077));
#18443=CARTESIAN_POINT('Ctrl Pts',(147.616192453019,-84.3176124815105,33.0537033222415));
#18444=CARTESIAN_POINT('Ctrl Pts',(147.612723530195,-84.3236850001122,33.0518963231399));
#18445=CARTESIAN_POINT('Ctrl Pts',(147.414398057485,-84.6708634135347,32.9485864574506));
#18446=CARTESIAN_POINT('Ctrl Pts',(147.213653682843,-85.0194306321787,32.8611210650963));
#18447=CARTESIAN_POINT('Ctrl Pts',(147.010609976479,-85.3690841855062,32.78802258227));
#18448=CARTESIAN_POINT('Ctrl Pts',(146.970506380411,-85.4381450055505,32.7735847448165));
#18449=CARTESIAN_POINT('Ctrl Pts',(146.930313102768,-85.5072481940713,32.7597072133851));
#18450=CARTESIAN_POINT('Ctrl Pts',(146.89003109062,-85.5763914060563,32.746378371904));
#18451=CARTESIAN_POINT('Ctrl Pts',(146.887290932544,-85.5810948287668,32.745471685999));
#18452=CARTESIAN_POINT('Ctrl Pts',(146.884550362083,-85.5857984397406,32.7445675390721));
#18453=CARTESIAN_POINT('Ctrl Pts',(146.881809379355,-85.5905022385503,32.7436659274155));
#18454=CARTESIAN_POINT('Ctrl Pts',(146.534412670975,-86.1866695207185,32.6293941669531));
#18455=CARTESIAN_POINT('Ctrl Pts',(146.180413916128,-86.7858240348916,32.5551812170606));
#18456=CARTESIAN_POINT('Ctrl Pts',(145.819603406855,-87.3878896742938,32.5213077186522));
#18457=CARTESIAN_POINT('Ctrl Pts',(145.668377266016,-87.6402328318194,32.5071103538045));
#18458=CARTESIAN_POINT('Ctrl Pts',(145.515954394551,-87.8930873961367,32.5000000002681));
#18459=CARTESIAN_POINT('Ctrl Pts',(145.36231884058,-88.1464478086873,32.5));
#18460=CARTESIAN_POINT('Origin',(0.,0.,32.5));
#18461=CARTESIAN_POINT('',(-145.36231884058,-88.1464478086873,-49.5));
#18462=CARTESIAN_POINT('Origin',(0.,0.,-49.5));
#18463=CARTESIAN_POINT('',(-150.289855072464,-79.4541343310581,-44.5));
#18464=CARTESIAN_POINT('Ctrl Pts',(-145.36231884058,-88.1464478086873,-49.5));
#18465=CARTESIAN_POINT('Ctrl Pts',(-145.729245608051,-87.5413488274995,
-49.4999999993448));
#18466=CARTESIAN_POINT('Ctrl Pts',(-146.089427497743,-86.938852139224,-49.459451627546));
#18467=CARTESIAN_POINT('Ctrl Pts',(-146.443059008834,-86.3390437438767,
-49.3785345234731));
#18468=CARTESIAN_POINT('Ctrl Pts',(-146.591729818533,-86.0868773022461,
-49.3445160296351));
#18469=CARTESIAN_POINT('Ctrl Pts',(-146.739242767663,-85.8351860376504,
-49.3033619016674));
#18470=CARTESIAN_POINT('Ctrl Pts',(-146.885611849037,-85.5839764893769,
-49.2550827834563));
#18471=CARTESIAN_POINT('Ctrl Pts',(-146.887215711036,-85.581223821639,-49.2545537575016));
#18472=CARTESIAN_POINT('Ctrl Pts',(-146.888819435246,-85.5784712124141,
-49.2540238618083));
#18473=CARTESIAN_POINT('Ctrl Pts',(-146.890423021642,-85.5757186617924,
-49.2534930956204));
#18474=CARTESIAN_POINT('Ctrl Pts',(-147.136163003217,-85.1539068149984,
-49.1721563659123));
#18475=CARTESIAN_POINT('Ctrl Pts',(-147.378654044698,-84.733492627337,-49.0703840441395));
#18476=CARTESIAN_POINT('Ctrl Pts',(-147.617771548819,-84.3148475830954,
-48.9454703779811));
#18477=CARTESIAN_POINT('Ctrl Pts',(-147.619992196193,-84.3109596911514,
-48.9443103240332));
#18478=CARTESIAN_POINT('Ctrl Pts',(-147.622212556282,-84.307071941363,-48.943148258573));
#18479=CARTESIAN_POINT('Ctrl Pts',(-147.624432625828,-84.303184339794,-48.9419841796181));
#18480=CARTESIAN_POINT('Ctrl Pts',(-147.797445356911,-84.0002188016352,
-48.8512660849843));
#18481=CARTESIAN_POINT('Ctrl Pts',(-147.968707326118,-83.6981287755317,
-48.7483109143164));
#18482=CARTESIAN_POINT('Ctrl Pts',(-148.136615104019,-83.3998939012959,
-48.6322285684957));
#18483=CARTESIAN_POINT('Ctrl Pts',(-148.200188500854,-83.2869759397415,
-48.5882773642776));
#18484=CARTESIAN_POINT('Ctrl Pts',(-148.263281189795,-83.1746104678287,
-48.5424447848479));
#18485=CARTESIAN_POINT('Ctrl Pts',(-148.325806750807,-83.0629583612551,
-48.4946842709289));
#18486=CARTESIAN_POINT('Ctrl Pts',(-148.328437713,-83.0582602431345,-48.4926745951353));
#18487=CARTESIAN_POINT('Ctrl Pts',(-148.331067922545,-83.0535629380485,
-48.4906613522023));
#18488=CARTESIAN_POINT('Ctrl Pts',(-148.333697371916,-83.0488664605796,
-48.4886445330394));
#18489=CARTESIAN_POINT('Ctrl Pts',(-148.479392264376,-82.7886398186652,
-48.3768948053783));
#18490=CARTESIAN_POINT('Ctrl Pts',(-148.622808981178,-82.5308543489962,
-48.2541267340886));
#18491=CARTESIAN_POINT('Ctrl Pts',(-148.762663381336,-82.2779954776877,
-48.1187795814413));
#18492=CARTESIAN_POINT('Ctrl Pts',(-148.840976563632,-82.1364040593145,
-48.0429902875284));
#18493=CARTESIAN_POINT('Ctrl Pts',(-148.918172933796,-81.9963571587517,
-47.9632574413117));
#18494=CARTESIAN_POINT('Ctrl Pts',(-148.994029023493,-81.8582880066048,
-47.8793133555439));
#18495=CARTESIAN_POINT('Ctrl Pts',(-148.996712266487,-81.8534041128184,
-47.8763440174079));
#18496=CARTESIAN_POINT('Ctrl Pts',(-148.999393672824,-81.8485229853453,
-47.8733697901463));
#18497=CARTESIAN_POINT('Ctrl Pts',(-149.002073232327,-81.8436446453373,
-47.8703906395336));
#18498=CARTESIAN_POINT('Ctrl Pts',(-149.107681065302,-81.6513776267181,
-47.7529752061311));
#18499=CARTESIAN_POINT('Ctrl Pts',(-149.210443318177,-81.4633981454557,
-47.6279048759376));
#18500=CARTESIAN_POINT('Ctrl Pts',(-149.309720948425,-81.2810297213993,
-47.4931045485117));
#18501=CARTESIAN_POINT('Ctrl Pts',(-149.401996350024,-81.111524068145,-47.3678119290385));
#18502=CARTESIAN_POINT('Ctrl Pts',(-149.491261252891,-80.9468661107977,
-47.2341131033335));
#18503=CARTESIAN_POINT('Ctrl Pts',(-149.577013895448,-80.7880986852943,
-47.0903818425147));
#18504=CARTESIAN_POINT('Ctrl Pts',(-149.583521150904,-80.7760507744081,
-47.0794749362875));
#18505=CARTESIAN_POINT('Ctrl Pts',(-149.590008187584,-80.7640367723622,
-47.0685102812695));
#18506=CARTESIAN_POINT('Ctrl Pts',(-149.596474789369,-80.752057129177,-47.0574871779499));
#18507=CARTESIAN_POINT('Ctrl Pts',(-149.598641974416,-80.7480423306098,
-47.0537929494384));
#18508=CARTESIAN_POINT('Ctrl Pts',(-149.600807137209,-80.7440308818109,
-47.050091283938));
#18509=CARTESIAN_POINT('Ctrl Pts',(-149.602970226706,-80.7400228807506,
-47.0463821931637));
#18510=CARTESIAN_POINT('Ctrl Pts',(-149.665071318886,-80.6249554072859,
-46.9398962671819));
#18511=CARTESIAN_POINT('Ctrl Pts',(-149.72550325001,-80.5126559819617,-46.8272204519951));
#18512=CARTESIAN_POINT('Ctrl Pts',(-149.783030801752,-80.4054929778246,
-46.7086718150296));
#18513=CARTESIAN_POINT('Ctrl Pts',(-149.809543928151,-80.3561040122254,
-46.6540354729443));
#18514=CARTESIAN_POINT('Ctrl Pts',(-149.835440369712,-80.3078056559303,
-46.5981521261349));
#18515=CARTESIAN_POINT('Ctrl Pts',(-149.860600799428,-80.260826858675,-46.5410549251661));
#18516=CARTESIAN_POINT('Ctrl Pts',(-149.862244464557,-80.2577578566065,
-46.5373249142225));
#18517=CARTESIAN_POINT('Ctrl Pts',(-149.863885113163,-80.2546942576169,
-46.5335897131967));
#18518=CARTESIAN_POINT('Ctrl Pts',(-149.865522721631,-80.2516361085815,
-46.5298492852785));
#18519=CARTESIAN_POINT('Ctrl Pts',(-149.920874283176,-80.148269932952,-46.4034219187085));
#18520=CARTESIAN_POINT('Ctrl Pts',(-149.972772946679,-80.0510921736928,
-46.2709925001795));
#18521=CARTESIAN_POINT('Ctrl Pts',(-150.020328326584,-79.961871940831,-46.1310781770696));
#18522=CARTESIAN_POINT('Ctrl Pts',(-150.041423437799,-79.9222946997582,
-46.0690135229251));
#18523=CARTESIAN_POINT('Ctrl Pts',(-150.061664115444,-79.884282891071,-46.0054765146034));
#18524=CARTESIAN_POINT('Ctrl Pts',(-150.080973718749,-79.8479888765764,
-45.9403401621094));
#18525=CARTESIAN_POINT('Ctrl Pts',(-150.081910893431,-79.8462273783758,
-45.9371788262994));
#18526=CARTESIAN_POINT('Ctrl Pts',(-150.082845417364,-79.8444707888363,
-45.9340152250091));
#18527=CARTESIAN_POINT('Ctrl Pts',(-150.083777280819,-79.842719127427,-45.9308493494822));
#18528=CARTESIAN_POINT('Ctrl Pts',(-150.124316972743,-79.7665150295208,
-45.7931214259646));
#18529=CARTESIAN_POINT('Ctrl Pts',(-150.159836015379,-79.6996105779127,
-45.6510364734858));
#18530=CARTESIAN_POINT('Ctrl Pts',(-150.189536570941,-79.643601630539,-45.5038983003528));
#18531=CARTESIAN_POINT('Ctrl Pts',(-150.205994764956,-79.6125649679259,
-45.4223635090175));
#18532=CARTESIAN_POINT('Ctrl Pts',(-150.22066665991,-79.5848732537911,-45.3392772231722));
#18533=CARTESIAN_POINT('Ctrl Pts',(-150.233419649245,-79.5607919801431,
-45.2545226584932));
#18534=CARTESIAN_POINT('Ctrl Pts',(-150.233653158554,-79.5603510481059,
-45.252970788629));
#18535=CARTESIAN_POINT('Ctrl Pts',(-150.233885994755,-79.5599113833124,
-45.2514181977489));
#18536=CARTESIAN_POINT('Ctrl Pts',(-150.234118156878,-79.5594729876405,
-45.2498648923104));
#18537=CARTESIAN_POINT('Ctrl Pts',(-150.243593980634,-79.5415796290569,
-45.1864658831964));
#18538=CARTESIAN_POINT('Ctrl Pts',(-150.251930637624,-79.5258311439937,
-45.1219886580334));
#18539=CARTESIAN_POINT('Ctrl Pts',(-150.25908694937,-79.5123085902624,-45.0567119030525));
#18540=CARTESIAN_POINT('Ctrl Pts',(-150.266133192886,-79.4989940212598,
-44.9924391424681));
#18541=CARTESIAN_POINT('Ctrl Pts',(-150.272035277524,-79.4878371314994,
-44.9273898861929));
#18542=CARTESIAN_POINT('Ctrl Pts',(-150.276731655023,-79.4789572453975,
-44.8618164804335));
#18543=CARTESIAN_POINT('Ctrl Pts',(-150.281154338818,-79.4705948579246,
-44.8000645367055));
#18544=CARTESIAN_POINT('Ctrl Pts',(-150.284507727575,-79.4642518495708,
-44.7378467346804));
#18545=CARTESIAN_POINT('Ctrl Pts',(-150.286719886614,-79.4600667280322,
-44.6753785307951));
#18546=CARTESIAN_POINT('Ctrl Pts',(-150.28878458935,-79.4561605749315,-44.6170742817893));
#18547=CARTESIAN_POINT('Ctrl Pts',(-150.289855072332,-79.4541343313065,
-44.5585512837797));
#18548=CARTESIAN_POINT('Ctrl Pts',(-150.289855072464,-79.4541343310581,
-44.5));
#18549=CARTESIAN_POINT('',(-150.289855072464,-79.4541343310581,-37.5));
#18550=CARTESIAN_POINT('',(-150.289855072464,-79.4541343310581,115.));
#18551=CARTESIAN_POINT('',(-145.36231884058,-88.1464478086873,-32.5));
#18552=CARTESIAN_POINT('Ctrl Pts',(-150.289855072464,-79.4541343310581,
-37.5));
#18553=CARTESIAN_POINT('Ctrl Pts',(-150.289855068577,-79.4541343384106,
-37.2436476198539));
#18554=CARTESIAN_POINT('Ctrl Pts',(-150.270581238553,-79.4906188049207,
-36.9946184779967));
#18555=CARTESIAN_POINT('Ctrl Pts',(-150.234400310691,-79.5589401936912,
-36.751988357395));
#18556=CARTESIAN_POINT('Ctrl Pts',(-150.23399376631,-79.559707882038,-36.7492620615819));
#18557=CARTESIAN_POINT('Ctrl Pts',(-150.2335850823,-79.5604795994251,-36.7465365450195));
#18558=CARTESIAN_POINT('Ctrl Pts',(-150.233174261933,-79.5612553394198,
-36.7438118068126));
#18559=CARTESIAN_POINT('Ctrl Pts',(-150.211108362071,-79.6029217279729,
-36.597461223358));
#18560=CARTESIAN_POINT('Ctrl Pts',(-150.183223768892,-79.6555340182885,
-36.4560333918963));
#18561=CARTESIAN_POINT('Ctrl Pts',(-150.150657295691,-79.7168744976241,
-36.3199679230369));
#18562=CARTESIAN_POINT('Ctrl Pts',(-150.129869982242,-79.756028377234,-36.233116776054));
#18563=CARTESIAN_POINT('Ctrl Pts',(-150.107175698488,-79.7987372956008,
-36.1484502339904));
#18564=CARTESIAN_POINT('Ctrl Pts',(-150.082875014062,-79.8444151271605,
-36.0660801928029));
#18565=CARTESIAN_POINT('Ctrl Pts',(-150.081600916097,-79.8468100404559,
-36.0617614872067));
#18566=CARTESIAN_POINT('Ctrl Pts',(-150.080322360849,-79.8492131928936,
-36.0574489500027));
#18567=CARTESIAN_POINT('Ctrl Pts',(-150.079039391808,-79.8516244996438,
-36.0531426012594));
#18568=CARTESIAN_POINT('Ctrl Pts',(-150.044542112236,-79.9164612341789,
-35.9373507841183));
#18569=CARTESIAN_POINT('Ctrl Pts',(-150.006537123414,-79.9877842267191,
-35.8251345497657));
#18570=CARTESIAN_POINT('Ctrl Pts',(-149.96597080498,-80.0637685558382,-35.7172653705196));
#18571=CARTESIAN_POINT('Ctrl Pts',(-149.933351576501,-80.1248672773407,
-35.6305281574933));
#18572=CARTESIAN_POINT('Ctrl Pts',(-149.899077126288,-80.188978256752,-35.5466015582195));
#18573=CARTESIAN_POINT('Ctrl Pts',(-149.863649966461,-80.2551332464107,
-35.4658772780747));
#18574=CARTESIAN_POINT('Ctrl Pts',(-149.861515024356,-80.259119935537,-35.4610126017813));
#18575=CARTESIAN_POINT('Ctrl Pts',(-149.85937578758,-80.2631142503696,-35.4561592869359));
#18576=CARTESIAN_POINT('Ctrl Pts',(-149.857232364154,-80.267115982567,-35.4513174183969));
#18577=CARTESIAN_POINT('Ctrl Pts',(-149.804252858374,-80.3660277475268,
-35.3316398039859));
#18578=CARTESIAN_POINT('Ctrl Pts',(-149.748484158681,-80.4699094426787,
-35.2180933723342));
#18579=CARTESIAN_POINT('Ctrl Pts',(-149.690355248213,-80.57789654445,-35.1097499754482));
#18580=CARTESIAN_POINT('Ctrl Pts',(-149.661473306623,-80.6315510365229,
-35.0559184545164));
#18581=CARTESIAN_POINT('Ctrl Pts',(-149.63200898684,-80.6862185043787,-35.0033707290548));
#18582=CARTESIAN_POINT('Ctrl Pts',(-149.60201639041,-80.741790230842,-34.9519894923051));
#18583=CARTESIAN_POINT('Ctrl Pts',(-149.599223408299,-80.7469652025476,
-34.9472047489958));
#18584=CARTESIAN_POINT('Ctrl Pts',(-149.596425806469,-80.7521480873936,
-34.9424300694399));
#18585=CARTESIAN_POINT('Ctrl Pts',(-149.593623625112,-80.7573388040449,
-34.9376653528747));
#18586=CARTESIAN_POINT('Ctrl Pts',(-149.503321107799,-80.9246137661054,
-34.7841185815493));
#18587=CARTESIAN_POINT('Ctrl Pts',(-149.407759531995,-81.1009468141073,
-34.6404004213243));
#18588=CARTESIAN_POINT('Ctrl Pts',(-149.309404815744,-81.2816192446487,
-34.5068550549154));
#18589=CARTESIAN_POINT('Ctrl Pts',(-149.306147321137,-81.2876030905756,
-34.5024320508386));
#18590=CARTESIAN_POINT('Ctrl Pts',(-149.302886794892,-81.293591637219,-34.4980202481262));
#18591=CARTESIAN_POINT('Ctrl Pts',(-149.299623326396,-81.2995847135541,
-34.4936196571968));
#18592=CARTESIAN_POINT('Ctrl Pts',(-149.201294060242,-81.4801578671635,
-34.3610285574967));
#18593=CARTESIAN_POINT('Ctrl Pts',(-149.100390942177,-81.6646756184357,
-34.2385852650972));
#18594=CARTESIAN_POINT('Ctrl Pts',(-148.997297013874,-81.8523394986246,
-34.1242886774832));
#18595=CARTESIAN_POINT('Ctrl Pts',(-148.993783486671,-81.8587352404398,
-34.1203933542915));
#18596=CARTESIAN_POINT('Ctrl Pts',(-148.99026742009,-81.8651346268366,-34.1165075135219));
#18597=CARTESIAN_POINT('Ctrl Pts',(-148.986748829868,-81.8715376251531,
-34.112631076538));
#18598=CARTESIAN_POINT('Ctrl Pts',(-148.828989574134,-82.1586219928198,
-33.9388274293518));
#18599=CARTESIAN_POINT('Ctrl Pts',(-148.666197521396,-82.4528887056537,
-33.783734495542));
#18600=CARTESIAN_POINT('Ctrl Pts',(-148.499047679152,-82.7528397831901,
-33.6438439889596));
#18601=CARTESIAN_POINT('Ctrl Pts',(-148.443888609357,-82.851822960194,-33.5976804382634));
#18602=CARTESIAN_POINT('Ctrl Pts',(-148.388255041158,-82.9514250552998,
-33.5531719910385));
#18603=CARTESIAN_POINT('Ctrl Pts',(-148.332171389768,-83.0515919680529,
-33.5101914075093));
#18604=CARTESIAN_POINT('Ctrl Pts',(-148.328463625565,-83.0582141348389,
-33.5073499044134));
#18605=CARTESIAN_POINT('Ctrl Pts',(-148.324753888106,-83.0648387811287,
-33.504515085708));
#18606=CARTESIAN_POINT('Ctrl Pts',(-148.321042184227,-83.0714658916727,
-33.5016869147109));
#18607=CARTESIAN_POINT('Ctrl Pts',(-148.12752607943,-83.4169817680272,-33.3542353256577));
#18608=CARTESIAN_POINT('Ctrl Pts',(-147.928023778942,-83.7703038875428,
-33.224894934649));
#18609=CARTESIAN_POINT('Ctrl Pts',(-147.726117191057,-84.1248695150572,
-33.1128740238486));
#18610=CARTESIAN_POINT('Ctrl Pts',(-147.691851026728,-84.1850438966121,
-33.0938626236858));
#18611=CARTESIAN_POINT('Ctrl Pts',(-147.657515670366,-84.24525399004,-33.0753500432682));
#18612=CARTESIAN_POINT('Ctrl Pts',(-147.623128700903,-84.3054675885418,
-33.0573323830855));
#18613=CARTESIAN_POINT('Ctrl Pts',(-147.61966084937,-84.3115399997815,-33.0555153410065));
#18614=CARTESIAN_POINT('Ctrl Pts',(-147.616192453019,-84.3176124815102,
-33.0537033222403));
#18615=CARTESIAN_POINT('Ctrl Pts',(-147.612723530195,-84.323685000112,-33.0518963231388));
#18616=CARTESIAN_POINT('Ctrl Pts',(-147.414398058157,-84.6708634123572,
-32.948586457801));
#18617=CARTESIAN_POINT('Ctrl Pts',(-147.213653684205,-85.0194306298146,
-32.8611210656896));
#18618=CARTESIAN_POINT('Ctrl Pts',(-147.010609978545,-85.3690841819489,
-32.7880225830139));
#18619=CARTESIAN_POINT('Ctrl Pts',(-146.970506381792,-85.4381450031775,
-32.7735847452933));
#18620=CARTESIAN_POINT('Ctrl Pts',(-146.93031310346,-85.5072481928842,-32.7597072136142));
#18621=CARTESIAN_POINT('Ctrl Pts',(-146.89003109062,-85.5763914060563,-32.7463783719042));
#18622=CARTESIAN_POINT('Ctrl Pts',(-146.887290932544,-85.5810948287669,
-32.7454716859993));
#18623=CARTESIAN_POINT('Ctrl Pts',(-146.884550362083,-85.5857984397407,
-32.7445675390723));
#18624=CARTESIAN_POINT('Ctrl Pts',(-146.881809379355,-85.5905022385503,
-32.7436659274158));
#18625=CARTESIAN_POINT('Ctrl Pts',(-146.53441266257,-86.186669535143,-32.6293941641891));
#18626=CARTESIAN_POINT('Ctrl Pts',(-146.180413898998,-86.7858240638849,
-32.5551812134692));
#18627=CARTESIAN_POINT('Ctrl Pts',(-145.819603380665,-87.3878897179948,
-32.5213077161934));
#18628=CARTESIAN_POINT('Ctrl Pts',(-145.668377248418,-87.6402328610125,
-32.5071103529836));
#18629=CARTESIAN_POINT('Ctrl Pts',(-145.515954385683,-87.8930874107624,
-32.5000000002681));
#18630=CARTESIAN_POINT('Ctrl Pts',(-145.36231884058,-88.1464478086873,-32.5));
#18631=CARTESIAN_POINT('Origin',(0.,0.,-32.5));
#18632=CARTESIAN_POINT('',(-119.689439203101,-120.724637681159,115.));
#18633=CARTESIAN_POINT('',(-145.36231884058,-88.1464478086873,32.5));
#18634=CARTESIAN_POINT('Origin',(0.,0.,32.5));
#18635=CARTESIAN_POINT('',(-150.289855072464,-79.4541343310581,37.5));
#18636=CARTESIAN_POINT('Ctrl Pts',(-145.36231884058,-88.1464478086873,32.5));
#18637=CARTESIAN_POINT('Ctrl Pts',(-145.729245608041,-87.5413488275162,
32.5000000006552));
#18638=CARTESIAN_POINT('Ctrl Pts',(-146.089427497723,-86.9388521392574,
32.5405483724518));
#18639=CARTESIAN_POINT('Ctrl Pts',(-146.443059008805,-86.3390437439265,
32.6214654765202));
#18640=CARTESIAN_POINT('Ctrl Pts',(-146.591729818514,-86.0868773022792,
32.6554839703595));
#18641=CARTESIAN_POINT('Ctrl Pts',(-146.739242767653,-85.835186037667,32.6966380983294));
#18642=CARTESIAN_POINT('Ctrl Pts',(-146.885611849037,-85.5839764893769,
32.7449172165437));
#18643=CARTESIAN_POINT('Ctrl Pts',(-146.887215711036,-85.581223821639,32.7454462424984));
#18644=CARTESIAN_POINT('Ctrl Pts',(-146.888819435246,-85.5784712124141,
32.7459761381918));
#18645=CARTESIAN_POINT('Ctrl Pts',(-146.890423021642,-85.5757186617924,
32.7465069043797));
#18646=CARTESIAN_POINT('Ctrl Pts',(-147.136163003217,-85.1539068149984,
32.8278436340878));
#18647=CARTESIAN_POINT('Ctrl Pts',(-147.378654044698,-84.733492627337,32.9296159558605));
#18648=CARTESIAN_POINT('Ctrl Pts',(-147.617771548819,-84.3148475830954,
33.0545296220188));
#18649=CARTESIAN_POINT('Ctrl Pts',(-147.619992196193,-84.3109596911514,
33.0556896759668));
#18650=CARTESIAN_POINT('Ctrl Pts',(-147.622212556282,-84.307071941363,33.056851741427));
#18651=CARTESIAN_POINT('Ctrl Pts',(-147.624432625828,-84.303184339794,33.0580158203819));
#18652=CARTESIAN_POINT('Ctrl Pts',(-147.797445356911,-84.000218801635,33.1487339150158));
#18653=CARTESIAN_POINT('Ctrl Pts',(-147.968707326118,-83.6981287755313,
33.2516890856837));
#18654=CARTESIAN_POINT('Ctrl Pts',(-148.13661510402,-83.3998939012953,33.3677714315045));
#18655=CARTESIAN_POINT('Ctrl Pts',(-148.200188500854,-83.2869759397412,
33.4117226357226));
#18656=CARTESIAN_POINT('Ctrl Pts',(-148.263281189795,-83.1746104678285,
33.4575552151522));
#18657=CARTESIAN_POINT('Ctrl Pts',(-148.325806750807,-83.0629583612551,
33.5053157290711));
#18658=CARTESIAN_POINT('Ctrl Pts',(-148.328437713,-83.0582602431345,33.5073254048647));
#18659=CARTESIAN_POINT('Ctrl Pts',(-148.331067922545,-83.0535629380485,
33.5093386477977));
#18660=CARTESIAN_POINT('Ctrl Pts',(-148.333697371916,-83.0488664605796,
33.5113554669606));
#18661=CARTESIAN_POINT('Ctrl Pts',(-148.479392264378,-82.7886398186623,
33.6231051946229));
#18662=CARTESIAN_POINT('Ctrl Pts',(-148.622808981182,-82.5308543489905,
33.7458732659141));
#18663=CARTESIAN_POINT('Ctrl Pts',(-148.76266338134,-82.2779954776793,33.8812204185632));
#18664=CARTESIAN_POINT('Ctrl Pts',(-148.840976563635,-82.136404059309,33.9570097124747));
#18665=CARTESIAN_POINT('Ctrl Pts',(-148.918172933798,-81.996357158749,34.0367425586899));
#18666=CARTESIAN_POINT('Ctrl Pts',(-148.994029023493,-81.8582880066048,
34.1206866444561));
#18667=CARTESIAN_POINT('Ctrl Pts',(-148.996712266487,-81.8534041128184,
34.1236559825921));
#18668=CARTESIAN_POINT('Ctrl Pts',(-148.999393672824,-81.8485229853453,
34.1266302098537));
#18669=CARTESIAN_POINT('Ctrl Pts',(-149.002073232327,-81.8436446453373,
34.1296093604664));
#18670=CARTESIAN_POINT('Ctrl Pts',(-149.107681065302,-81.6513776267181,
34.2470247938689));
#18671=CARTESIAN_POINT('Ctrl Pts',(-149.210443318177,-81.4633981454557,
34.3720951240624));
#18672=CARTESIAN_POINT('Ctrl Pts',(-149.309720948425,-81.2810297213993,
34.5068954514883));
#18673=CARTESIAN_POINT('Ctrl Pts',(-149.401996350023,-81.1115240681461,
34.6321880709607));
#18674=CARTESIAN_POINT('Ctrl Pts',(-149.49126125289,-80.9468661107998,34.7658868966648));
#18675=CARTESIAN_POINT('Ctrl Pts',(-149.577013895446,-80.7880986852974,
34.9096181574825));
#18676=CARTESIAN_POINT('Ctrl Pts',(-149.583521150902,-80.7760507744102,
34.9205250637106));
#18677=CARTESIAN_POINT('Ctrl Pts',(-149.590008187584,-80.7640367723632,
34.9314897187296));
#18678=CARTESIAN_POINT('Ctrl Pts',(-149.596474789369,-80.752057129177,34.9425128220501));
#18679=CARTESIAN_POINT('Ctrl Pts',(-149.598641974416,-80.7480423306098,
34.9462070505616));
#18680=CARTESIAN_POINT('Ctrl Pts',(-149.600807137209,-80.7440308818109,
34.949908716062));
#18681=CARTESIAN_POINT('Ctrl Pts',(-149.602970226706,-80.7400228807506,
34.9536178068363));
#18682=CARTESIAN_POINT('Ctrl Pts',(-149.665071318885,-80.6249554072882,
35.060103732816));
#18683=CARTESIAN_POINT('Ctrl Pts',(-149.725503250007,-80.5126559819663,
35.1727795480004));
#18684=CARTESIAN_POINT('Ctrl Pts',(-149.783030801748,-80.4054929778311,
35.2913281849631));
#18685=CARTESIAN_POINT('Ctrl Pts',(-149.809543928148,-80.3561040122296,
35.3459645270507));
#18686=CARTESIAN_POINT('Ctrl Pts',(-149.835440369711,-80.3078056559324,
35.4018478738626));
#18687=CARTESIAN_POINT('Ctrl Pts',(-149.860600799428,-80.260826858675,35.4589450748339));
#18688=CARTESIAN_POINT('Ctrl Pts',(-149.862244464557,-80.2577578566065,
35.4626750857775));
#18689=CARTESIAN_POINT('Ctrl Pts',(-149.863885113163,-80.2546942576169,
35.4664102868033));
#18690=CARTESIAN_POINT('Ctrl Pts',(-149.865522721631,-80.2516361085815,
35.4701507147215));
#18691=CARTESIAN_POINT('Ctrl Pts',(-149.920874283176,-80.1482699329536,
35.5965780812897));
#18692=CARTESIAN_POINT('Ctrl Pts',(-149.972772946677,-80.0510921736956,
35.7290074998166));
#18693=CARTESIAN_POINT('Ctrl Pts',(-150.020328326582,-79.961871940835,35.8689218229242));
#18694=CARTESIAN_POINT('Ctrl Pts',(-150.041423437798,-79.9222946997607,
35.9309864770707));
#18695=CARTESIAN_POINT('Ctrl Pts',(-150.061664115444,-79.8842828910722,
35.9945234853944));
#18696=CARTESIAN_POINT('Ctrl Pts',(-150.080973718749,-79.8479888765764,
36.0596598378906));
#18697=CARTESIAN_POINT('Ctrl Pts',(-150.081910893431,-79.8462273783758,
36.0628211737006));
#18698=CARTESIAN_POINT('Ctrl Pts',(-150.082845417364,-79.8444707888363,
36.0659847749909));
#18699=CARTESIAN_POINT('Ctrl Pts',(-150.083777280819,-79.842719127427,36.0691506505178));
#18700=CARTESIAN_POINT('Ctrl Pts',(-150.124316972746,-79.7665150295156,
36.2068785740447));
#18701=CARTESIAN_POINT('Ctrl Pts',(-150.159836015384,-79.6996105779036,
36.3489635265334));
#18702=CARTESIAN_POINT('Ctrl Pts',(-150.189536570947,-79.6436016305276,
36.4961016996771));
#18703=CARTESIAN_POINT('Ctrl Pts',(-150.205994764959,-79.6125649679192,
36.5776364910029));
#18704=CARTESIAN_POINT('Ctrl Pts',(-150.220666659912,-79.5848732537881,
36.6607227768382));
#18705=CARTESIAN_POINT('Ctrl Pts',(-150.233419649245,-79.5607919801431,
36.7454773415068));
#18706=CARTESIAN_POINT('Ctrl Pts',(-150.233653158554,-79.5603510481059,
36.747029211371));
#18707=CARTESIAN_POINT('Ctrl Pts',(-150.233885994755,-79.5599113833124,
36.7485818022511));
#18708=CARTESIAN_POINT('Ctrl Pts',(-150.234118156878,-79.5594729876405,
36.7501351076896));
#18709=CARTESIAN_POINT('Ctrl Pts',(-150.243593980634,-79.541579629057,36.8135341168033));
#18710=CARTESIAN_POINT('Ctrl Pts',(-150.251930637624,-79.5258311439938,
36.8780113419661));
#18711=CARTESIAN_POINT('Ctrl Pts',(-150.25908694937,-79.5123085902626,36.9432880969467));
#18712=CARTESIAN_POINT('Ctrl Pts',(-150.266133192885,-79.49899402126,37.0075608575309));
#18713=CARTESIAN_POINT('Ctrl Pts',(-150.272035277523,-79.4878371314996,
37.0726101138059));
#18714=CARTESIAN_POINT('Ctrl Pts',(-150.276731655023,-79.4789572453977,
37.1381835195651));
#18715=CARTESIAN_POINT('Ctrl Pts',(-150.281154338818,-79.4705948579248,
37.1999354632931));
#18716=CARTESIAN_POINT('Ctrl Pts',(-150.284507727575,-79.4642518495709,
37.2621532653183));
#18717=CARTESIAN_POINT('Ctrl Pts',(-150.286719886614,-79.4600667280323,
37.3246214692037));
#18718=CARTESIAN_POINT('Ctrl Pts',(-150.28878458935,-79.4561605749315,37.3829257182099));
#18719=CARTESIAN_POINT('Ctrl Pts',(-150.289855072332,-79.4541343313065,
37.4414487162198));
#18720=CARTESIAN_POINT('Ctrl Pts',(-150.289855072464,-79.4541343310581,
37.5));
#18721=CARTESIAN_POINT('',(-150.289855072464,-79.4541343310581,44.5));
#18722=CARTESIAN_POINT('',(-150.289855072464,-79.4541343310581,115.));
#18723=CARTESIAN_POINT('',(-145.36231884058,-88.1464478086873,49.5));
#18724=CARTESIAN_POINT('Ctrl Pts',(-150.289855072464,-79.4541343310581,
44.5));
#18725=CARTESIAN_POINT('Ctrl Pts',(-150.289855068577,-79.4541343384106,
44.7563523801461));
#18726=CARTESIAN_POINT('Ctrl Pts',(-150.270581238553,-79.4906188049207,
45.0053815220034));
#18727=CARTESIAN_POINT('Ctrl Pts',(-150.23440031069,-79.5589401936918,45.2480116426047));
#18728=CARTESIAN_POINT('Ctrl Pts',(-150.233993766309,-79.5597078820386,
45.2507379384179));
#18729=CARTESIAN_POINT('Ctrl Pts',(-150.2335850823,-79.5604795994257,45.2534634549803));
#18730=CARTESIAN_POINT('Ctrl Pts',(-150.233174261933,-79.5612553394204,
45.2561881931872));
#18731=CARTESIAN_POINT('Ctrl Pts',(-150.211108362005,-79.6029217280976,
45.4025387770759));
#18732=CARTESIAN_POINT('Ctrl Pts',(-150.183223768725,-79.6555340186023,
45.5439666089425));
#18733=CARTESIAN_POINT('Ctrl Pts',(-150.1506572954,-79.7168744981717,45.6800320781738));
#18734=CARTESIAN_POINT('Ctrl Pts',(-150.129869982031,-79.7560283776325,
45.7668832247325));
#18735=CARTESIAN_POINT('Ctrl Pts',(-150.107175698374,-79.7987372958143,
45.8515497663918));
#18736=CARTESIAN_POINT('Ctrl Pts',(-150.082875014061,-79.8444151271613,
45.9339198071965));
#18737=CARTESIAN_POINT('Ctrl Pts',(-150.081600916097,-79.8468100404567,
45.9382385127928));
#18738=CARTESIAN_POINT('Ctrl Pts',(-150.080322360848,-79.8492131928944,
45.9425510499967));
#18739=CARTESIAN_POINT('Ctrl Pts',(-150.079039391808,-79.8516244996445,
45.94685739874));
#18740=CARTESIAN_POINT('Ctrl Pts',(-150.044542112121,-79.9164612343949,
46.0626492162668));
#18741=CARTESIAN_POINT('Ctrl Pts',(-150.006537123161,-79.9877842271942,
46.1748654509807));
#18742=CARTESIAN_POINT('Ctrl Pts',(-149.965970804575,-80.0637685565973,
46.2827346305569));
#18743=CARTESIAN_POINT('Ctrl Pts',(-149.933351576217,-80.1248672778719,
46.3694718432009));
#18744=CARTESIAN_POINT('Ctrl Pts',(-149.899077126141,-80.1889782570263,
46.4533984421142));
#18745=CARTESIAN_POINT('Ctrl Pts',(-149.863649966461,-80.2551332464111,
46.5341227219249));
#18746=CARTESIAN_POINT('Ctrl Pts',(-149.861515024356,-80.2591199355374,
46.5389873982183));
#18747=CARTESIAN_POINT('Ctrl Pts',(-149.85937578758,-80.2631142503699,46.5438407130638));
#18748=CARTESIAN_POINT('Ctrl Pts',(-149.857232364154,-80.2671159825673,
46.5486825816028));
#18749=CARTESIAN_POINT('Ctrl Pts',(-149.804252858279,-80.3660277477057,
46.6683601962307));
#18750=CARTESIAN_POINT('Ctrl Pts',(-149.748484158479,-80.4699094430547,
46.7819066280769));
#18751=CARTESIAN_POINT('Ctrl Pts',(-149.690355247898,-80.5778965450365,
46.8902500251402));
#18752=CARTESIAN_POINT('Ctrl Pts',(-149.661473306408,-80.6315510369212,
46.9440815458665));
#18753=CARTESIAN_POINT('Ctrl Pts',(-149.632008986731,-80.6862185045812,
46.9966292711324));
#18754=CARTESIAN_POINT('Ctrl Pts',(-149.60201639041,-80.741790230842,47.0480105076949));
#18755=CARTESIAN_POINT('Ctrl Pts',(-149.599223408299,-80.7469652025476,
47.0527952510041));
#18756=CARTESIAN_POINT('Ctrl Pts',(-149.596425806469,-80.7521480873936,
47.0575699305601));
#18757=CARTESIAN_POINT('Ctrl Pts',(-149.593623625112,-80.7573388040449,
47.0623346471253));
#18758=CARTESIAN_POINT('Ctrl Pts',(-149.503321107799,-80.9246137661054,
47.2158814184506));
#18759=CARTESIAN_POINT('Ctrl Pts',(-149.407759531995,-81.1009468141059,
47.3595995786781));
#18760=CARTESIAN_POINT('Ctrl Pts',(-149.309404815745,-81.2816192446479,
47.4931449450858));
#18761=CARTESIAN_POINT('Ctrl Pts',(-149.306147321137,-81.2876030905749,
47.4975679491626));
#18762=CARTESIAN_POINT('Ctrl Pts',(-149.302886794892,-81.2935916372183,
47.501979751875));
#18763=CARTESIAN_POINT('Ctrl Pts',(-149.299623326396,-81.2995847135535,
47.5063803428043));
#18764=CARTESIAN_POINT('Ctrl Pts',(-149.201294060241,-81.4801578671638,
47.6389714425028));
#18765=CARTESIAN_POINT('Ctrl Pts',(-149.100390942177,-81.6646756184357,
47.7614147349028));
#18766=CARTESIAN_POINT('Ctrl Pts',(-148.997297013874,-81.8523394986245,
47.8757113225169));
#18767=CARTESIAN_POINT('Ctrl Pts',(-148.993783486671,-81.8587352404397,
47.8796066457086));
#18768=CARTESIAN_POINT('Ctrl Pts',(-148.99026742009,-81.8651346268366,47.8834924864782));
#18769=CARTESIAN_POINT('Ctrl Pts',(-148.986748829868,-81.871537625153,47.8873689234621));
#18770=CARTESIAN_POINT('Ctrl Pts',(-148.828989572841,-82.1586219951734,
48.0611725720732));
#18771=CARTESIAN_POINT('Ctrl Pts',(-148.666197518726,-82.4528887104789,
48.2162655070009));
#18772=CARTESIAN_POINT('Ctrl Pts',(-148.499047675041,-82.7528397905676,
48.3561560144813));
#18773=CARTESIAN_POINT('Ctrl Pts',(-148.443888606593,-82.851822965143,48.4023195639484));
#18774=CARTESIAN_POINT('Ctrl Pts',(-148.388255039765,-82.9514250577883,
48.4468280100297));
#18775=CARTESIAN_POINT('Ctrl Pts',(-148.332171389768,-83.0515919680528,
48.4898085924912));
#18776=CARTESIAN_POINT('Ctrl Pts',(-148.328463625565,-83.0582141348388,
48.4926500955871));
#18777=CARTESIAN_POINT('Ctrl Pts',(-148.324753888106,-83.0648387811285,
48.4954849142925));
#18778=CARTESIAN_POINT('Ctrl Pts',(-148.321042184227,-83.0714658916725,
48.4983130852896));
#18779=CARTESIAN_POINT('Ctrl Pts',(-148.127526079489,-83.4169817679216,
48.6457646742983));
#18780=CARTESIAN_POINT('Ctrl Pts',(-147.928023779063,-83.7703038873281,
48.7751050652708));
#18781=CARTESIAN_POINT('Ctrl Pts',(-147.726117191241,-84.1248695147338,
48.8871259760477));
#18782=CARTESIAN_POINT('Ctrl Pts',(-147.691851026851,-84.1850438963965,
48.9061373762463));
#18783=CARTESIAN_POINT('Ctrl Pts',(-147.657515670427,-84.2452539899323,
48.9246499566981));
#18784=CARTESIAN_POINT('Ctrl Pts',(-147.623128700903,-84.3054675885421,
48.9426676169133));
#18785=CARTESIAN_POINT('Ctrl Pts',(-147.61966084937,-84.3115399997817,48.9444846589923));
#18786=CARTESIAN_POINT('Ctrl Pts',(-147.616192453019,-84.3176124815105,
48.9462966777585));
#18787=CARTESIAN_POINT('Ctrl Pts',(-147.612723530195,-84.3236850001122,
48.9481036768601));
#18788=CARTESIAN_POINT('Ctrl Pts',(-147.41439805748,-84.6708634135425,49.0514135425518));
#18789=CARTESIAN_POINT('Ctrl Pts',(-147.213653682834,-85.0194306321946,
49.1388789349076));
#18790=CARTESIAN_POINT('Ctrl Pts',(-147.010609976465,-85.3690841855301,
49.211977417735));
#18791=CARTESIAN_POINT('Ctrl Pts',(-146.970506380402,-85.4381450055664,
49.2264152551867));
#18792=CARTESIAN_POINT('Ctrl Pts',(-146.930313102763,-85.5072481940793,
49.2402927866165));
#18793=CARTESIAN_POINT('Ctrl Pts',(-146.89003109062,-85.5763914060563,49.253621628096));
#18794=CARTESIAN_POINT('Ctrl Pts',(-146.887290932544,-85.5810948287668,
49.254528314001));
#18795=CARTESIAN_POINT('Ctrl Pts',(-146.884550362083,-85.5857984397406,
49.2554324609279));
#18796=CARTESIAN_POINT('Ctrl Pts',(-146.881809379355,-85.5905022385503,
49.2563340725845));
#18797=CARTESIAN_POINT('Ctrl Pts',(-146.534412670951,-86.18666952076,49.3706058330548));
#18798=CARTESIAN_POINT('Ctrl Pts',(-146.180413916078,-86.7858240349752,
49.4448187829498));
#18799=CARTESIAN_POINT('Ctrl Pts',(-145.819603406779,-87.3878896744197,
49.4786922813549));
#18800=CARTESIAN_POINT('Ctrl Pts',(-145.668377265966,-87.6402328319036,
49.4928896461978));
#18801=CARTESIAN_POINT('Ctrl Pts',(-145.515954394526,-87.8930873961788,
49.4999999997319));
#18802=CARTESIAN_POINT('Ctrl Pts',(-145.36231884058,-88.1464478086873,49.5));
#18803=CARTESIAN_POINT('Origin',(0.,0.,49.5));
#18804=CARTESIAN_POINT('',(-119.689439203101,-120.724637681159,82.5));
#18805=CARTESIAN_POINT('',(-119.689439203101,-120.724637681159,115.));
#18806=CARTESIAN_POINT('',(-114.505594583524,-125.652173913043,87.5));
#18807=CARTESIAN_POINT('Ctrl Pts',(-114.505594583524,-125.652173913043,
87.5));
#18808=CARTESIAN_POINT('Ctrl Pts',(-114.875320870893,-125.315245971011,
87.4999999999648));
#18809=CARTESIAN_POINT('Ctrl Pts',(-115.240344827216,-124.979614114477,
87.4659613720207));
#18810=CARTESIAN_POINT('Ctrl Pts',(-115.600645981712,-124.645458541841,
87.3949999559647));
#18811=CARTESIAN_POINT('Ctrl Pts',(-115.815592858116,-124.446109481549,
87.3526661068053));
#18812=CARTESIAN_POINT('Ctrl Pts',(-116.028858884767,-124.247285605303,
87.2971925583144));
#18813=CARTESIAN_POINT('Ctrl Pts',(-116.240439697973,-124.049023288465,
87.2279752537405));
#18814=CARTESIAN_POINT('Ctrl Pts',(-116.245828883255,-124.043973339257,
87.2262122163769));
#18815=CARTESIAN_POINT('Ctrl Pts',(-116.251215926061,-124.038924730883,
87.2244403150215));
#18816=CARTESIAN_POINT('Ctrl Pts',(-116.25660079453,-124.033877495354,87.2226595463959));
#18817=CARTESIAN_POINT('Ctrl Pts',(-116.416321749011,-123.884171094794,
87.1698400455657));
#18818=CARTESIAN_POINT('Ctrl Pts',(-116.574127438346,-123.735675041936,
87.1092235235697));
#18819=CARTESIAN_POINT('Ctrl Pts',(-116.729307012311,-123.589109583791,
87.0406588491595));
#18820=CARTESIAN_POINT('Ctrl Pts',(-116.845631220869,-123.479242605265,
86.9892620623144));
#18821=CARTESIAN_POINT('Ctrl Pts',(-116.960479920838,-123.370460219089,
86.9333980875197));
#18822=CARTESIAN_POINT('Ctrl Pts',(-117.073550031386,-123.263067798316,
86.8729844025496));
#18823=CARTESIAN_POINT('Ctrl Pts',(-117.079344844513,-123.257563965281,
86.8698882172442));
#18824=CARTESIAN_POINT('Ctrl Pts',(-117.085135613102,-123.252063194138,
86.866779947454));
#18825=CARTESIAN_POINT('Ctrl Pts',(-117.090922329314,-123.24656549557,86.8636595351634));
#18826=CARTESIAN_POINT('Ctrl Pts',(-117.252833947861,-123.092740555707,
86.7763507773263));
#18827=CARTESIAN_POINT('Ctrl Pts',(-117.41152726411,-122.94136441611,86.6795632238393));
#18828=CARTESIAN_POINT('Ctrl Pts',(-117.56661345365,-122.792879292928,86.5721870844521));
#18829=CARTESIAN_POINT('Ctrl Pts',(-117.663683594914,-122.699940831253,
86.5049791850918));
#18830=CARTESIAN_POINT('Ctrl Pts',(-117.759340859086,-122.608134753002,
86.4336238696885));
#18831=CARTESIAN_POINT('Ctrl Pts',(-117.853493006743,-122.517566847009,
86.3578587588989));
#18832=CARTESIAN_POINT('Ctrl Pts',(-117.859134880481,-122.512139751579,
86.3533186905155));
#18833=CARTESIAN_POINT('Ctrl Pts',(-117.864772463519,-122.506716022107,
86.3487614273767));
#18834=CARTESIAN_POINT('Ctrl Pts',(-117.870405487109,-122.50129592327,86.3441871089973));
#18835=CARTESIAN_POINT('Ctrl Pts',(-117.971986956633,-122.403554169484,
86.2616974876393));
#18836=CARTESIAN_POINT('Ctrl Pts',(-118.07218659958,-122.306895851518,86.1735699087692));
#18837=CARTESIAN_POINT('Ctrl Pts',(-118.16934447046,-122.212953361598,86.0806804467646));
#18838=CARTESIAN_POINT('Ctrl Pts',(-118.186308138277,-122.196551096106,
86.0644620389012));
#18839=CARTESIAN_POINT('Ctrl Pts',(-118.203179139119,-122.180231567871,
86.0480985650011));
#18840=CARTESIAN_POINT('Ctrl Pts',(-118.219948731942,-122.164003379953,
86.0315948052611));
#18841=CARTESIAN_POINT('Ctrl Pts',(-118.225239204071,-122.158883710274,
86.0263881981678));
#18842=CARTESIAN_POINT('Ctrl Pts',(-118.2305200644,-122.153772676115,86.0211674735436));
#18843=CARTESIAN_POINT('Ctrl Pts',(-118.235791265575,-122.148670330441,
86.0159325934032));
#18844=CARTESIAN_POINT('Ctrl Pts',(-118.348386205055,-122.039682211169,
85.9041134855647));
#18845=CARTESIAN_POINT('Ctrl Pts',(-118.456626331103,-121.93460772812,85.7857889099975));
#18846=CARTESIAN_POINT('Ctrl Pts',(-118.560193282322,-121.833823583021,
85.6604137446068));
#18847=CARTESIAN_POINT('Ctrl Pts',(-118.564867100718,-121.829275348417,
85.6547557547994));
#18848=CARTESIAN_POINT('Ctrl Pts',(-118.569531415015,-121.824735838064,
85.649083428181));
#18849=CARTESIAN_POINT('Ctrl Pts',(-118.57418617698,-121.820205105343,85.6433966843365));
#18850=CARTESIAN_POINT('Ctrl Pts',(-118.656113089353,-121.7404611903,85.5433062031976));
#18851=CARTESIAN_POINT('Ctrl Pts',(-118.735109022985,-121.663408950081,
85.438709891701));
#18852=CARTESIAN_POINT('Ctrl Pts',(-118.81085074319,-121.589398131885,85.3292725022672));
#18853=CARTESIAN_POINT('Ctrl Pts',(-118.830778159308,-121.569926110818,
85.3004798581036));
#18854=CARTESIAN_POINT('Ctrl Pts',(-118.850480457644,-121.550664485438,
85.2713523136863));
#18855=CARTESIAN_POINT('Ctrl Pts',(-118.869952060987,-121.531619330202,
85.2418842081897));
#18856=CARTESIAN_POINT('Ctrl Pts',(-118.873852582751,-121.527804233869,
85.2359812024218));
#18857=CARTESIAN_POINT('Ctrl Pts',(-118.87774476105,-121.523996924348,85.2300626384257));
#18858=CARTESIAN_POINT('Ctrl Pts',(-118.881628379448,-121.520197619565,
85.2241287426542));
#18859=CARTESIAN_POINT('Ctrl Pts',(-118.953933356783,-121.449462388129,
85.1136518225954));
#18860=CARTESIAN_POINT('Ctrl Pts',(-119.023372190228,-121.381403002907,
84.9976861670382));
#18861=CARTESIAN_POINT('Ctrl Pts',(-119.088533293315,-121.317439625798,
84.8776565982512));
#18862=CARTESIAN_POINT('Ctrl Pts',(-119.107675671495,-121.298649103596,
84.8423955101238));
#18863=CARTESIAN_POINT('Ctrl Pts',(-119.126449080996,-121.280211875355,
84.8067838787667));
#18864=CARTESIAN_POINT('Ctrl Pts',(-119.144818331366,-121.262163368406,
84.7708581772729));
#18865=CARTESIAN_POINT('Ctrl Pts',(-119.147770180269,-121.259263061406,
84.7650850923405));
#18866=CARTESIAN_POINT('Ctrl Pts',(-119.150711776641,-121.256372617005,
84.7593040201353));
#18867=CARTESIAN_POINT('Ctrl Pts',(-119.153643085904,-121.253492073365,
84.7535149461629));
#18868=CARTESIAN_POINT('Ctrl Pts',(-119.217477211424,-121.190763453585,
84.6274482498874));
#18869=CARTESIAN_POINT('Ctrl Pts',(-119.276475877676,-121.132687812754,
84.497494707205));
#18870=CARTESIAN_POINT('Ctrl Pts',(-119.330291692485,-121.079649407418,
84.3634783756072));
#18871=CARTESIAN_POINT('Ctrl Pts',(-119.344664771969,-121.065483957758,
84.3276854141313));
#18872=CARTESIAN_POINT('Ctrl Pts',(-119.358668331276,-121.051677644484,
84.2916027835783));
#18873=CARTESIAN_POINT('Ctrl Pts',(-119.37229615525,-121.038237390605,84.2552274353945));
#18874=CARTESIAN_POINT('Ctrl Pts',(-119.374201887271,-121.036357888622,
84.2501406610181));
#18875=CARTESIAN_POINT('Ctrl Pts',(-119.376100550482,-121.034485269244,
84.2450470253995));
#18876=CARTESIAN_POINT('Ctrl Pts',(-119.377992089409,-121.032619589192,
84.2399466200188));
#18877=CARTESIAN_POINT('Ctrl Pts',(-119.432704267988,-120.978655370584,
84.0924189715063));
#18878=CARTESIAN_POINT('Ctrl Pts',(-119.481511542447,-120.930442075982,
83.9390510932854));
#18879=CARTESIAN_POINT('Ctrl Pts',(-119.523061427328,-120.889361770029,
83.7819751614297));
#18880=CARTESIAN_POINT('Ctrl Pts',(-119.53066769299,-120.88184146711,83.7532202979645));
#18881=CARTESIAN_POINT('Ctrl Pts',(-119.538030846413,-120.874560108483,
83.7243411856524));
#18882=CARTESIAN_POINT('Ctrl Pts',(-119.545142732111,-120.867526032261,
83.6953509136308));
#18883=CARTESIAN_POINT('Ctrl Pts',(-119.546090881023,-120.866588256825,
83.6914859619103));
#18884=CARTESIAN_POINT('Ctrl Pts',(-119.547034430282,-120.865655009876,
83.6876198631647));
#18885=CARTESIAN_POINT('Ctrl Pts',(-119.547973377994,-120.864726293782,
83.6837526181086));
#18886=CARTESIAN_POINT('Ctrl Pts',(-119.593937460371,-120.819263077397,
83.4944402974945));
#18887=CARTESIAN_POINT('Ctrl Pts',(-119.62890424618,-120.784628102355,83.3022686788512));
#18888=CARTESIAN_POINT('Ctrl Pts',(-119.65264519197,-120.761105073466,83.1071682749086));
#18889=CARTESIAN_POINT('Ctrl Pts',(-119.676892336666,-120.737080492046,
82.9079079856867));
#18890=CARTESIAN_POINT('Ctrl Pts',(-119.689439200918,-120.724637683323,
82.7055895150371));
#18891=CARTESIAN_POINT('Ctrl Pts',(-119.689439203101,-120.724637681159,
82.5));
#18892=CARTESIAN_POINT('',(-102.653719754201,-135.507246376812,87.5));
#18893=CARTESIAN_POINT('Origin',(0.,0.,87.5));
#18894=CARTESIAN_POINT('',(-95.8022538025509,-140.434782608696,82.5));
#18895=CARTESIAN_POINT('Ctrl Pts',(-102.653719754201,-135.507246376812,
87.5));
#18896=CARTESIAN_POINT('Ctrl Pts',(-102.215883490062,-135.838929901929,
87.4999999991685));
#18897=CARTESIAN_POINT('Ctrl Pts',(-101.781087350657,-136.164971110003,
87.4669218367414));
#18898=CARTESIAN_POINT('Ctrl Pts',(-101.349415497286,-136.485515662914,
87.4008783684644));
#18899=CARTESIAN_POINT('Ctrl Pts',(-101.07973591123,-136.68577037414,87.3596188444822));
#18900=CARTESIAN_POINT('Ctrl Pts',(-100.811275778686,-136.88387961001,87.3054922341186));
#18901=CARTESIAN_POINT('Ctrl Pts',(-100.544056427545,-137.079877141377,
87.2385159157322));
#18902=CARTESIAN_POINT('Ctrl Pts',(-100.541162556084,-137.081999710944,
87.2377905908054));
#18903=CARTESIAN_POINT('Ctrl Pts',(-100.538268831608,-137.084122031661,
87.2370637322218));
#18904=CARTESIAN_POINT('Ctrl Pts',(-100.535375254373,-137.086244103409,
87.2363353381554));
#18905=CARTESIAN_POINT('Ctrl Pts',(-100.190565643195,-137.339118201716,
87.1495371453096));
#18906=CARTESIAN_POINT('Ctrl Pts',(-99.8478512789412,-137.588453369916,
87.040933511602));
#18907=CARTESIAN_POINT('Ctrl Pts',(-99.5077977395583,-137.833951510589,
86.9074976668159));
#18908=CARTESIAN_POINT('Ctrl Pts',(-99.5037755731161,-137.836855272111,
86.9059193824726));
#18909=CARTESIAN_POINT('Ctrl Pts',(-99.4997536170413,-137.839758608548,
86.9043375053786));
#18910=CARTESIAN_POINT('Ctrl Pts',(-99.4957318889749,-137.842661507683,
86.9027520347699));
#18911=CARTESIAN_POINT('Ctrl Pts',(-99.2674376143156,-138.007445213001,
86.8127524483652));
#18912=CARTESIAN_POINT('Ctrl Pts',(-99.0398204570979,-138.170861151964,
86.711145683115));
#18913=CARTESIAN_POINT('Ctrl Pts',(-98.8161737755042,-138.33062666086,86.597820472154));
#18914=CARTESIAN_POINT('Ctrl Pts',(-98.7076262937751,-138.408169254089,
86.5428177948124));
#18915=CARTESIAN_POINT('Ctrl Pts',(-98.600013904115,-138.484852125992,86.4850552618045));
#18916=CARTESIAN_POINT('Ctrl Pts',(-98.4937108917853,-138.56041611792,86.4245237415767));
#18917=CARTESIAN_POINT('Ctrl Pts',(-98.4889708281906,-138.563785525046,
86.4218246341001));
#18918=CARTESIAN_POINT('Ctrl Pts',(-98.4842329483831,-138.56715301161,86.419119965262));
#18919=CARTESIAN_POINT('Ctrl Pts',(-98.479497264693,-138.570518570128,86.4164097092555));
#18920=CARTESIAN_POINT('Ctrl Pts',(-98.2490703748719,-138.73427849005,86.2845352212039));
#18921=CARTESIAN_POINT('Ctrl Pts',(-98.0238750005084,-138.8934512373,86.1394754931963));
#18922=CARTESIAN_POINT('Ctrl Pts',(-97.8050966305876,-139.047339894881,
85.9780962529129));
#18923=CARTESIAN_POINT('Ctrl Pts',(-97.7156206980972,-139.110277246236,
85.9120954045925));
#18924=CARTESIAN_POINT('Ctrl Pts',(-97.6272183327067,-139.172330541299,
85.8433644738521));
#18925=CARTESIAN_POINT('Ctrl Pts',(-97.5399718160535,-139.233451074562,
85.7716868356771));
#18926=CARTESIAN_POINT('Ctrl Pts',(-97.5352562713784,-139.236754548629,
85.7678127657659));
#18927=CARTESIAN_POINT('Ctrl Pts',(-97.5305452293931,-139.240054504138,
85.7639310032341));
#18928=CARTESIAN_POINT('Ctrl Pts',(-97.5258387376046,-139.243350910624,
85.7600415156019));
#18929=CARTESIAN_POINT('Ctrl Pts',(-97.3552183240805,-139.362852710079,
85.6190392536152));
#18930=CARTESIAN_POINT('Ctrl Pts',(-97.1907405919816,-139.47757645948,85.4680354210839));
#18931=CARTESIAN_POINT('Ctrl Pts',(-97.0346910654179,-139.586057153202,
85.3056163231383));
#18932=CARTESIAN_POINT('Ctrl Pts',(-96.9159928871056,-139.668572371353,
85.1820731668481));
#18933=CARTESIAN_POINT('Ctrl Pts',(-96.8021704778946,-139.747475893107,
85.0519259141839));
#18934=CARTESIAN_POINT('Ctrl Pts',(-96.694215926304,-139.822132033515,84.9145642707921));
#18935=CARTESIAN_POINT('Ctrl Pts',(-96.6906380099125,-139.824606347239,
84.9100117209624));
#18936=CARTESIAN_POINT('Ctrl Pts',(-96.6870657587802,-139.827076536154,
84.9054498746293));
#18937=CARTESIAN_POINT('Ctrl Pts',(-96.6834992847061,-139.82954252561,84.9008787661799));
#18938=CARTESIAN_POINT('Ctrl Pts',(-96.5933790288425,-139.891854937294,
84.7853726796454));
#18939=CARTESIAN_POINT('Ctrl Pts',(-96.5068951547278,-139.951522102754,
84.6638795752373));
#18940=CARTESIAN_POINT('Ctrl Pts',(-96.4259038292281,-140.007303114121,
84.5370163776214));
#18941=CARTESIAN_POINT('Ctrl Pts',(-96.3961160047755,-140.027818829404,
84.4903573232502));
#18942=CARTESIAN_POINT('Ctrl Pts',(-96.3670708290736,-140.047809094726,
84.4429721152884));
#18943=CARTESIAN_POINT('Ctrl Pts',(-96.3388592767016,-140.067213127358,
84.3948922769621));
#18944=CARTESIAN_POINT('Ctrl Pts',(-96.3362565453866,-140.069003297665,
84.390456544423));
#18945=CARTESIAN_POINT('Ctrl Pts',(-96.3336613068006,-140.070788207782,
84.3860158118469));
#18946=CARTESIAN_POINT('Ctrl Pts',(-96.3310735989047,-140.072567833443,
84.3815700581723));
#18947=CARTESIAN_POINT('Ctrl Pts',(-96.2565223686416,-140.123838412584,
84.2534889844106));
#18948=CARTESIAN_POINT('Ctrl Pts',(-96.18818677241,-140.170746863762,84.1211671345774));
#18949=CARTESIAN_POINT('Ctrl Pts',(-96.126962800212,-140.212720695597,83.9840977199587));
#18950=CARTESIAN_POINT('Ctrl Pts',(-96.1019843048262,-140.229845412064,
83.9281753807562));
#18951=CARTESIAN_POINT('Ctrl Pts',(-96.0781891189942,-140.246149048065,
83.8714630194104));
#18952=CARTESIAN_POINT('Ctrl Pts',(-96.0556361395659,-140.261594051371,
83.8139272219729));
#18953=CARTESIAN_POINT('Ctrl Pts',(-96.0542034790336,-140.262575183231,
83.8102723050498));
#18954=CARTESIAN_POINT('Ctrl Pts',(-96.0527757857576,-140.263552881361,
83.8066133446794));
#18955=CARTESIAN_POINT('Ctrl Pts',(-96.0513530943973,-140.264527122689,
83.802950400001));
#18956=CARTESIAN_POINT('Ctrl Pts',(-95.9866237488953,-140.308852972491,
83.6362944279056));
#18957=CARTESIAN_POINT('Ctrl Pts',(-95.9322125151014,-140.346047836819,
83.4612414093815));
#18958=CARTESIAN_POINT('Ctrl Pts',(-95.8913844101215,-140.373937837985,
83.2831693720156));
#18959=CARTESIAN_POINT('Ctrl Pts',(-95.883045620544,-140.379634131044,83.2467996886822));
#18960=CARTESIAN_POINT('Ctrl Pts',(-95.8752733682718,-140.384942326837,
83.2103039208797));
#18961=CARTESIAN_POINT('Ctrl Pts',(-95.8680953540231,-140.38984398165,83.1737276630787));
#18962=CARTESIAN_POINT('Ctrl Pts',(-95.8676809810245,-140.390126944783,
83.1716161858517));
#18963=CARTESIAN_POINT('Ctrl Pts',(-95.8672684958815,-140.390408616667,
83.1695042863138));
#18964=CARTESIAN_POINT('Ctrl Pts',(-95.8668579005401,-140.390688996011,
83.1673919642828));
#18965=CARTESIAN_POINT('Ctrl Pts',(-95.8468264218082,-140.404367701805,
83.0643393244232));
#18966=CARTESIAN_POINT('Ctrl Pts',(-95.8312774654238,-140.414980545424,
82.9601876791363));
#18967=CARTESIAN_POINT('Ctrl Pts',(-95.8204649814164,-140.422358778653,
82.855032721006));
#18968=CARTESIAN_POINT('Ctrl Pts',(-95.8099639220234,-140.429524501655,
82.7529064695304));
#18969=CARTESIAN_POINT('Ctrl Pts',(-95.8039305392802,-140.433639185389,
82.649833883227));
#18970=CARTESIAN_POINT('Ctrl Pts',(-95.8025570944415,-140.434575788992,
82.5459117712175));
#18971=CARTESIAN_POINT('Ctrl Pts',(-95.802355077537,-140.434713551904,82.5306261020837));
#18972=CARTESIAN_POINT('Ctrl Pts',(-95.8022538025544,-140.434782608693,
82.5153220699784));
#18973=CARTESIAN_POINT('Ctrl Pts',(-95.8022538025544,-140.434782608693,
82.5));
#18974=CARTESIAN_POINT('',(-95.8022538025509,-140.434782608696,-82.5));
#18975=CARTESIAN_POINT('',(-95.802253802551,-140.434782608696,115.));
#18976=CARTESIAN_POINT('',(-102.653719754201,-135.507246376812,-87.5));
#18977=CARTESIAN_POINT('Ctrl Pts',(-95.8022538025509,-140.434782608696,
-82.5));
#18978=CARTESIAN_POINT('Ctrl Pts',(-95.802253806658,-140.434782605894,-82.7267635628216));
#18979=CARTESIAN_POINT('Ctrl Pts',(-95.82442316008,-140.419665963906,-82.9488530674831));
#18980=CARTESIAN_POINT('Ctrl Pts',(-95.8667225776694,-140.39078140277,-83.1666939397165));
#18981=CARTESIAN_POINT('Ctrl Pts',(-95.8671957348732,-140.390458302857,
-83.1691306866946));
#18982=CARTESIAN_POINT('Ctrl Pts',(-95.8676714126208,-140.390133479021,
-83.1715669081132));
#18983=CARTESIAN_POINT('Ctrl Pts',(-95.8681496080969,-140.389806933124,
-83.1740026044675));
#18984=CARTESIAN_POINT('Ctrl Pts',(-95.9022176054039,-140.366542880454,
-83.347528497089));
#18985=CARTESIAN_POINT('Ctrl Pts',(-95.9496913058974,-140.334107437353,
-83.5193033103441));
#18986=CARTESIAN_POINT('Ctrl Pts',(-96.0075075764083,-140.294541978644,
-83.6842311536406));
#18987=CARTESIAN_POINT('Ctrl Pts',(-96.0214298424351,-140.285014542219,
-83.7239460866395));
#18988=CARTESIAN_POINT('Ctrl Pts',(-96.0359516723967,-140.275073772703,
-83.763263842758));
#18989=CARTESIAN_POINT('Ctrl Pts',(-96.0510300136253,-140.264748363786,
-83.8021130045776));
#18990=CARTESIAN_POINT('Ctrl Pts',(-96.0526816582041,-140.263617343775,
-83.8063684466409));
#18991=CARTESIAN_POINT('Ctrl Pts',(-96.0543400150297,-140.262481684736,
-83.8106183997866));
#18992=CARTESIAN_POINT('Ctrl Pts',(-96.0560050279566,-140.261341424076,
-83.8148627669174));
#18993=CARTESIAN_POINT('Ctrl Pts',(-96.1087379306465,-140.22522803811,-83.9492868277003));
#18994=CARTESIAN_POINT('Ctrl Pts',(-96.1682453864427,-140.18443183692,-84.0791983701216));
#18995=CARTESIAN_POINT('Ctrl Pts',(-96.2337564928184,-140.139445304685,
-84.2050184597015));
#18996=CARTESIAN_POINT('Ctrl Pts',(-96.2645815930236,-140.118277682266,
-84.2642208924444));
#18997=CARTESIAN_POINT('Ctrl Pts',(-96.2967352970674,-140.096182731474,
-84.3225177941468));
#18998=CARTESIAN_POINT('Ctrl Pts',(-96.3301343379528,-140.073213779952,
-84.379954552556));
#18999=CARTESIAN_POINT('Ctrl Pts',(-96.3331813229761,-140.071118329022,
-84.3851944917284));
#19000=CARTESIAN_POINT('Ctrl Pts',(-96.3362387534725,-140.069015548404,
-84.3904274269311));
#19001=CARTESIAN_POINT('Ctrl Pts',(-96.339306565948,-140.066905478751,-84.395653391359));
#19002=CARTESIAN_POINT('Ctrl Pts',(-96.4117861971074,-140.017053321434,
-84.519121164313));
#19003=CARTESIAN_POINT('Ctrl Pts',(-96.4899842015251,-139.963182743773,
-84.6383213996312));
#19004=CARTESIAN_POINT('Ctrl Pts',(-96.5721307818922,-139.90648063707,-84.7523713002298));
#19005=CARTESIAN_POINT('Ctrl Pts',(-96.6081754743616,-139.881600599589,
-84.8024146930877));
#19006=CARTESIAN_POINT('Ctrl Pts',(-96.6449798262798,-139.856175797233,
-84.8514667730734));
#19007=CARTESIAN_POINT('Ctrl Pts',(-96.6823922460858,-139.830307960496,
-84.8994546030547));
#19008=CARTESIAN_POINT('Ctrl Pts',(-96.6866911658693,-139.827335585128,
-84.9049687032585));
#19009=CARTESIAN_POINT('Ctrl Pts',(-96.6909982721163,-139.824357251049,
-84.9104689623343));
#19010=CARTESIAN_POINT('Ctrl Pts',(-96.6953133447443,-139.821373105703,
-84.9159552790218));
#19011=CARTESIAN_POINT('Ctrl Pts',(-96.8598715687415,-139.707570697129,
-85.1251796903365));
#19012=CARTESIAN_POINT('Ctrl Pts',(-97.0374177596496,-139.584350181588,
-85.3170893229325));
#19013=CARTESIAN_POINT('Ctrl Pts',(-97.2253643375751,-139.453317353096,
-85.4947229550121));
#19014=CARTESIAN_POINT('Ctrl Pts',(-97.32204057764,-139.385916492046,-85.5860944066665));
#19015=CARTESIAN_POINT('Ctrl Pts',(-97.4214682282139,-139.316448809721,
-85.6736891853026));
#19016=CARTESIAN_POINT('Ctrl Pts',(-97.5232920470755,-139.245134572953,
-85.757925116709));
#19017=CARTESIAN_POINT('Ctrl Pts',(-97.5293253469245,-139.240909037329,
-85.7629162930164));
#19018=CARTESIAN_POINT('Ctrl Pts',(-97.5353667088673,-139.236677264113,
-85.7678953452707));
#19019=CARTESIAN_POINT('Ctrl Pts',(-97.5414160595539,-139.232439298911,
-85.7728623680754));
#19020=CARTESIAN_POINT('Ctrl Pts',(-97.7162996213869,-139.109921943276,
-85.916456397384));
#19021=CARTESIAN_POINT('Ctrl Pts',(-97.895291385601,-138.984032327335,-86.0478104717196));
#19022=CARTESIAN_POINT('Ctrl Pts',(-98.0778068955091,-138.855116179076,
-86.1688889209447));
#19023=CARTESIAN_POINT('Ctrl Pts',(-98.2081021472136,-138.763084756681,
-86.2553251203982));
#19024=CARTESIAN_POINT('Ctrl Pts',(-98.3401938137772,-138.669510448868,
-86.3365230931734));
#19025=CARTESIAN_POINT('Ctrl Pts',(-98.473875270995,-138.57451383921,-86.4131838583186));
#19026=CARTESIAN_POINT('Ctrl Pts',(-98.4804799835183,-138.569820403706,
-86.4169713867174));
#19027=CARTESIAN_POINT('Ctrl Pts',(-98.4870884834129,-138.565123562489,
-86.4207477533706));
#19028=CARTESIAN_POINT('Ctrl Pts',(-98.4937007396705,-138.560423334432,
-86.4245130392829));
#19029=CARTESIAN_POINT('Ctrl Pts',(-98.7840182381348,-138.354055281161,
-86.589831554546));
#19030=CARTESIAN_POINT('Ctrl Pts',(-99.0816753104982,-138.141093446353,
-86.7335191028593));
#19031=CARTESIAN_POINT('Ctrl Pts',(-99.3855316162202,-137.922137712459,
-86.8583876011185));
#19032=CARTESIAN_POINT('Ctrl Pts',(-99.4178327914482,-137.898861817259,
-86.8716616361369));
#19033=CARTESIAN_POINT('Ctrl Pts',(-99.4502040159161,-137.875518191501,
-86.8847230529014));
#19034=CARTESIAN_POINT('Ctrl Pts',(-99.4826439161488,-137.852107558311,
-86.8975752625188));
#19035=CARTESIAN_POINT('Ctrl Pts',(-99.48920062357,-137.847375833759,-86.9001729332136));
#19036=CARTESIAN_POINT('Ctrl Pts',(-99.4957601913218,-137.842641332283,
-86.9027620700696));
#19037=CARTESIAN_POINT('Ctrl Pts',(-99.5023226100945,-137.83790405835,-86.9053427012605));
#19038=CARTESIAN_POINT('Ctrl Pts',(-99.7610782418026,-137.65111373735,-87.0070967765687));
#19039=CARTESIAN_POINT('Ctrl Pts',(-100.023540548839,-137.460524429142,
-87.0951230471669));
#19040=CARTESIAN_POINT('Ctrl Pts',(-100.286778083675,-137.268209582455,
-87.1698025082003));
#19041=CARTESIAN_POINT('Ctrl Pts',(-100.367689288363,-137.209097853065,
-87.1927567011173));
#19042=CARTESIAN_POINT('Ctrl Pts',(-100.448673514677,-137.149823232022,
-87.2144496897515));
#19043=CARTESIAN_POINT('Ctrl Pts',(-100.529644945651,-137.09044635394,-87.23489188421));
#19044=CARTESIAN_POINT('Ctrl Pts',(-100.535236887058,-137.08634574686,-87.2363036358892));
#19045=CARTESIAN_POINT('Ctrl Pts',(-100.54082877009,-137.082244650117,-87.237709423426));
#19046=CARTESIAN_POINT('Ctrl Pts',(-100.546420565381,-137.078143084482,
-87.2391092499));
#19047=CARTESIAN_POINT('Ctrl Pts',(-101.006759432587,-136.740485859902,
-87.3543485424286));
#19048=CARTESIAN_POINT('Ctrl Pts',(-101.469785375605,-136.39729021652,-87.4312211202132));
#19049=CARTESIAN_POINT('Ctrl Pts',(-101.935255327548,-136.048534047702,
-87.470101040684));
#19050=CARTESIAN_POINT('Ctrl Pts',(-102.174111258821,-135.869569800617,
-87.490052273998));
#19051=CARTESIAN_POINT('Ctrl Pts',(-102.413610624815,-135.689141411486,
-87.4999999996522));
#19052=CARTESIAN_POINT('Ctrl Pts',(-102.653719754201,-135.507246376812,
-87.5000000000001));
#19053=CARTESIAN_POINT('',(-114.505594583524,-125.652173913043,-87.5));
#19054=CARTESIAN_POINT('Origin',(0.,0.,-87.5));
#19055=CARTESIAN_POINT('',(-119.689439203101,-120.724637681159,-82.5));
#19056=CARTESIAN_POINT('Ctrl Pts',(-119.689439203101,-120.724637681159,
-82.5));
#19057=CARTESIAN_POINT('Ctrl Pts',(-119.689439202152,-120.7246376821,-82.7035326184388));
#19058=CARTESIAN_POINT('Ctrl Pts',(-119.677137855384,-120.736837058147,
-82.9047280297057));
#19059=CARTESIAN_POINT('Ctrl Pts',(-119.653068783703,-120.760685368386,
-83.1036884565072));
#19060=CARTESIAN_POINT('Ctrl Pts',(-119.653066214652,-120.760687913874,
-83.1037096928655));
#19061=CARTESIAN_POINT('Ctrl Pts',(-119.653063645461,-120.7606904595,-83.1037309292184));
#19062=CARTESIAN_POINT('Ctrl Pts',(-119.65306107613,-120.760693005266,-83.1037521655657));
#19063=CARTESIAN_POINT('Ctrl Pts',(-119.641919852122,-120.771732040813,
-83.1958379461839));
#19064=CARTESIAN_POINT('Ctrl Pts',(-119.628149514844,-120.785373482746,
-83.2877525621625));
#19065=CARTESIAN_POINT('Ctrl Pts',(-119.611957511397,-120.801406080513,
-83.3788351080295));
#19066=CARTESIAN_POINT('Ctrl Pts',(-119.594967539087,-120.818228791367,
-83.4744063532567));
#19067=CARTESIAN_POINT('Ctrl Pts',(-119.575311134826,-120.837684355012,
-83.5690634421961));
#19068=CARTESIAN_POINT('Ctrl Pts',(-119.553189137567,-120.859567147534,
-83.6620443506994));
#19069=CARTESIAN_POINT('Ctrl Pts',(-119.55083740086,-120.861893454956,-83.6719289290666));
#19070=CARTESIAN_POINT('Ctrl Pts',(-119.548457767033,-120.86424722548,-83.6817945487908));
#19071=CARTESIAN_POINT('Ctrl Pts',(-119.546050454752,-120.866628234349,
-83.6916402803605));
#19072=CARTESIAN_POINT('Ctrl Pts',(-119.545706019787,-120.866968905858,
-83.6930489942345));
#19073=CARTESIAN_POINT('Ctrl Pts',(-119.545361019709,-120.867310133486,
-83.6944572963284));
#19074=CARTESIAN_POINT('Ctrl Pts',(-119.545015455303,-120.867651916433,
-83.695865183348));
#19075=CARTESIAN_POINT('Ctrl Pts',(-119.498574793915,-120.913584384681,
-83.8850721826734));
#19076=CARTESIAN_POINT('Ctrl Pts',(-119.442053836954,-120.969435426432,
-84.0677448259361));
#19077=CARTESIAN_POINT('Ctrl Pts',(-119.376325844471,-121.034263033589,
-84.2444400249407));
#19078=CARTESIAN_POINT('Ctrl Pts',(-119.375341514619,-121.035233879443,
-84.2470861784687));
#19079=CARTESIAN_POINT('Ctrl Pts',(-119.374355124208,-121.036206734212,
-84.2497309822518));
#19080=CARTESIAN_POINT('Ctrl Pts',(-119.373366676025,-121.037181594878,
-84.2523744389033));
#19081=CARTESIAN_POINT('Ctrl Pts',(-119.316775771429,-121.092994583215,
-84.4037183391141));
#19082=CARTESIAN_POINT('Ctrl Pts',(-119.253023740241,-121.155791267692,
-84.5514088438984));
#19083=CARTESIAN_POINT('Ctrl Pts',(-119.183533814918,-121.224111669973,
-84.6934551425812));
#19084=CARTESIAN_POINT('Ctrl Pts',(-119.172587065958,-121.234874183951,
-84.7158316981047));
#19085=CARTESIAN_POINT('Ctrl Pts',(-119.161497891799,-121.245773805399,
-84.7380680949191));
#19086=CARTESIAN_POINT('Ctrl Pts',(-119.150271823512,-121.256804856299,
-84.7601564357346));
#19087=CARTESIAN_POINT('Ctrl Pts',(-119.148539861699,-121.25850673076,-84.7635642328206));
#19088=CARTESIAN_POINT('Ctrl Pts',(-119.146804666256,-121.260211709207,
-84.7669684593406));
#19089=CARTESIAN_POINT('Ctrl Pts',(-119.14506625839,-121.261919769914,-84.7703690853655));
#19090=CARTESIAN_POINT('Ctrl Pts',(-119.003325690235,-121.401185991481,
-85.0476381166482));
#19091=CARTESIAN_POINT('Ctrl Pts',(-118.842142596216,-121.559065359909,
-85.2991641553159));
#19092=CARTESIAN_POINT('Ctrl Pts',(-118.664609127849,-121.732125899566,
-85.5295567869234));
#19093=CARTESIAN_POINT('Ctrl Pts',(-118.633782041256,-121.762176302405,
-85.5695623907698));
#19094=CARTESIAN_POINT('Ctrl Pts',(-118.602462012018,-121.792684378039,
-85.6089309023198));
#19095=CARTESIAN_POINT('Ctrl Pts',(-118.570665287738,-121.82363207749,-85.6476865935965));
#19096=CARTESIAN_POINT('Ctrl Pts',(-118.567733597814,-121.826485486471,
-85.6512599072689));
#19097=CARTESIAN_POINT('Ctrl Pts',(-118.564797840986,-121.829342646821,
-85.6548280160802));
#19098=CARTESIAN_POINT('Ctrl Pts',(-118.561858031783,-121.832203542636,
-85.6583909367595));
#19099=CARTESIAN_POINT('Ctrl Pts',(-118.462775020542,-121.928626865597,
-85.778475229769));
#19100=CARTESIAN_POINT('Ctrl Pts',(-118.358568312162,-122.029796767798,
-85.8929376096802));
#19101=CARTESIAN_POINT('Ctrl Pts',(-118.251586150404,-122.133379331252,
-86.0001705886231));
#19102=CARTESIAN_POINT('Ctrl Pts',(-118.244181406579,-122.140548772723,
-86.0075926926972));
#19103=CARTESIAN_POINT('Ctrl Pts',(-118.236763379045,-122.147729760661,
-86.0149801731508));
#19104=CARTESIAN_POINT('Ctrl Pts',(-118.229332851436,-122.154921516527,
-86.0223325018978));
#19105=CARTESIAN_POINT('Ctrl Pts',(-118.226055490992,-122.158093562638,
-86.025575371406));
#19106=CARTESIAN_POINT('Ctrl Pts',(-118.222775639178,-122.161267761231,
-86.0288114700423));
#19107=CARTESIAN_POINT('Ctrl Pts',(-118.219493362288,-122.164444046394,
-86.0320407520766));
#19108=CARTESIAN_POINT('Ctrl Pts',(-118.104628229969,-122.27559993839,-86.1450512994916));
#19109=CARTESIAN_POINT('Ctrl Pts',(-117.986476048706,-122.389622505763,
-86.2501973510142));
#19110=CARTESIAN_POINT('Ctrl Pts',(-117.865390836685,-122.506120837556,
-86.3482582753084));
#19111=CARTESIAN_POINT('Ctrl Pts',(-117.861984025646,-122.509398593743,
-86.3510172830667));
#19112=CARTESIAN_POINT('Ctrl Pts',(-117.858574879434,-122.512678322681,
-86.3537706967463));
#19113=CARTESIAN_POINT('Ctrl Pts',(-117.855163404827,-122.515960016733,
-86.3565185352217));
#19114=CARTESIAN_POINT('Ctrl Pts',(-117.634786734593,-122.727953037703,
-86.5340252041163));
#19115=CARTESIAN_POINT('Ctrl Pts',(-117.404749948821,-122.948091205422,
-86.688414031018));
#19116=CARTESIAN_POINT('Ctrl Pts',(-117.165977845125,-123.175215067974,
-86.8223776503798));
#19117=CARTESIAN_POINT('Ctrl Pts',(-117.138194040773,-123.201643469212,
-86.837965815551));
#19118=CARTESIAN_POINT('Ctrl Pts',(-117.110291974294,-123.228166441777,
-86.8532774790446));
#19119=CARTESIAN_POINT('Ctrl Pts',(-117.082273113258,-123.25478214762,-86.8683169246712));
#19120=CARTESIAN_POINT('Ctrl Pts',(-117.079074540411,-123.257820539291,
-86.8700337954016));
#19121=CARTESIAN_POINT('Ctrl Pts',(-117.075874453949,-123.260860131433,
-86.8717471117034));
#19122=CARTESIAN_POINT('Ctrl Pts',(-117.072672856275,-123.263900921107,
-86.8734568798947));
#19123=CARTESIAN_POINT('Ctrl Pts',(-116.860769282127,-123.465161124843,
-86.9866210022035));
#19124=CARTESIAN_POINT('Ctrl Pts',(-116.644679584752,-123.669347667652,
-87.0827876682341));
#19125=CARTESIAN_POINT('Ctrl Pts',(-116.426318424243,-123.874581795949,
-87.1633254347002));
#19126=CARTESIAN_POINT('Ctrl Pts',(-116.366869236994,-123.930457126958,
-87.1852519748784));
#19127=CARTESIAN_POINT('Ctrl Pts',(-116.307251767595,-123.986410045268,
-87.2060203735688));
#19128=CARTESIAN_POINT('Ctrl Pts',(-116.247504799008,-124.042402536954,
-87.2256588635441));
#19129=CARTESIAN_POINT('Ctrl Pts',(-116.245124621172,-124.044633145315,
-87.2264412145098));
#19130=CARTESIAN_POINT('Ctrl Pts',(-116.242744233986,-124.046863820072,
-87.227221773433));
#19131=CARTESIAN_POINT('Ctrl Pts',(-116.24036363979,-124.049094558926,-87.228000542122));
#19132=CARTESIAN_POINT('Ctrl Pts',(-115.831177222972,-124.432523217204,
-87.3618585385571));
#19133=CARTESIAN_POINT('Ctrl Pts',(-115.413668066505,-124.8199443176,-87.4448575175416));
#19134=CARTESIAN_POINT('Ctrl Pts',(-114.988112144685,-125.210757527825,
-87.4801920420612));
#19135=CARTESIAN_POINT('Ctrl Pts',(-114.828401684543,-125.357429103603,
-87.4934530328749));
#19136=CARTESIAN_POINT('Ctrl Pts',(-114.667557747887,-125.504578468743,
-87.4999999998164));
#19137=CARTESIAN_POINT('Ctrl Pts',(-114.505594583524,-125.652173913044,
-87.5));
#19138=CARTESIAN_POINT('',(-119.689439203101,-120.724637681159,115.));
#19139=CARTESIAN_POINT('Origin',(-180.,-140.,85.));
#19140=CARTESIAN_POINT('',(-168.964466094067,-140.,-82.5));
#19141=CARTESIAN_POINT('',(-97.2111104761179,-140.,-82.5));
#19142=CARTESIAN_POINT('',(-180.,-140.,-82.5));
#19143=CARTESIAN_POINT('',(-97.2111104761179,-140.,82.5));
#19144=CARTESIAN_POINT('',(-97.2111104761179,-140.,85.));
#19145=CARTESIAN_POINT('',(-168.964466094067,-140.,82.5));
#19146=CARTESIAN_POINT('',(-170.,-140.,82.5));
#19147=CARTESIAN_POINT('',(-177.5,-140.,73.9644660940671));
#19148=CARTESIAN_POINT('',(-178.232233047034,-140.,73.2322330470335));
#19149=CARTESIAN_POINT('',(-177.5,-140.,-73.9644660940673));
#19150=CARTESIAN_POINT('',(-177.5,-140.,85.));
#19151=CARTESIAN_POINT('',(-168.232233047034,-140.,-83.2322330470337));
#19152=CARTESIAN_POINT('Origin',(-115.217186218029,-125.,85.));
#19153=CARTESIAN_POINT('',(-168.964466094067,-125.,-82.5));
#19154=CARTESIAN_POINT('',(-177.5,-125.,-73.9644660940673));
#19155=CARTESIAN_POINT('',(-178.232233047034,-125.,-73.2322330470336));
#19156=CARTESIAN_POINT('',(-177.5,-125.,73.9644660940672));
#19157=CARTESIAN_POINT('',(-177.5,-125.,85.));
#19158=CARTESIAN_POINT('',(-168.964466094067,-125.,82.5));
#19159=CARTESIAN_POINT('',(-168.232233047034,-125.,83.2322330470337));
#19160=CARTESIAN_POINT('',(-121.449578014911,-125.,82.5));
#19161=CARTESIAN_POINT('',(-115.217186218029,-125.,82.5));
#19162=CARTESIAN_POINT('',(-121.449578014911,-125.,47.));
#19163=CARTESIAN_POINT('',(-147.5,-125.,49.5));
#19164=CARTESIAN_POINT('',(-150.,-125.,49.5));
#19165=CARTESIAN_POINT('',(-152.5,-125.,44.5));
#19166=CARTESIAN_POINT('Origin',(-147.5,-125.,44.5));
#19167=CARTESIAN_POINT('',(-152.5,-125.,37.5));
#19168=CARTESIAN_POINT('',(-152.5,-125.,35.));
#19169=CARTESIAN_POINT('',(-147.5,-125.,32.5));
#19170=CARTESIAN_POINT('Origin',(-147.5,-125.,37.5));
#19171=CARTESIAN_POINT('',(-115.217186218029,-125.,32.5));
#19172=CARTESIAN_POINT('',(-121.449578014911,-125.,-35.));
#19173=CARTESIAN_POINT('',(-147.5,-125.,-32.5));
#19174=CARTESIAN_POINT('',(-115.217186218029,-125.,-32.5));
#19175=CARTESIAN_POINT('',(-152.5,-125.,-37.5));
#19176=CARTESIAN_POINT('Origin',(-147.5,-125.,-37.5));
#19177=CARTESIAN_POINT('',(-152.5,-125.,-44.5));
#19178=CARTESIAN_POINT('',(-152.5,-125.,85.));
#19179=CARTESIAN_POINT('',(-147.5,-125.,-49.5));
#19180=CARTESIAN_POINT('Origin',(-147.5,-125.,-44.5));
#19181=CARTESIAN_POINT('',(-115.217186218029,-125.,-49.5));
#19182=CARTESIAN_POINT('',(-121.449578014911,-125.,-82.5));
#19183=CARTESIAN_POINT('',(-121.449578014911,-125.,-85.));
#19184=CARTESIAN_POINT('',(-115.217186218029,-125.,-82.5));
#19185=CARTESIAN_POINT('Origin',(115.217186218029,-125.,85.));
#19186=CARTESIAN_POINT('',(147.5,-125.,49.5));
#19187=CARTESIAN_POINT('',(115.217186218029,-125.,49.5));
#19188=CARTESIAN_POINT('',(168.964466094067,-125.,82.5));
#19189=CARTESIAN_POINT('',(115.217186218029,-125.,82.5));
#19190=CARTESIAN_POINT('',(177.5,-125.,73.9644660940673));
#19191=CARTESIAN_POINT('',(140.840826156048,-125.,110.623639938019));
#19192=CARTESIAN_POINT('',(177.5,-125.,-73.9644660940672));
#19193=CARTESIAN_POINT('',(177.5,-125.,85.));
#19194=CARTESIAN_POINT('',(168.964466094067,-125.,-82.5));
#19195=CARTESIAN_POINT('',(225.840826156048,-125.,-25.623639938019));
#19196=CARTESIAN_POINT('',(115.217186218029,-125.,-82.5));
#19197=CARTESIAN_POINT('',(147.5,-125.,-49.5));
#19198=CARTESIAN_POINT('',(115.217186218029,-125.,-49.5));
#19199=CARTESIAN_POINT('',(152.5,-125.,-44.5));
#19200=CARTESIAN_POINT('Origin',(147.5,-125.,-44.5));
#19201=CARTESIAN_POINT('',(152.5,-125.,-37.5));
#19202=CARTESIAN_POINT('',(152.5,-125.,85.));
#19203=CARTESIAN_POINT('',(147.5,-125.,-32.5));
#19204=CARTESIAN_POINT('Origin',(147.5,-125.,-37.5));
#19205=CARTESIAN_POINT('',(115.217186218029,-125.,-32.5));
#19206=CARTESIAN_POINT('',(147.5,-125.,32.5));
#19207=CARTESIAN_POINT('',(150.,-125.,32.5));
#19208=CARTESIAN_POINT('',(152.5,-125.,37.5));
#19209=CARTESIAN_POINT('Origin',(147.5,-125.,37.5));
#19210=CARTESIAN_POINT('',(152.5,-125.,44.5));
#19211=CARTESIAN_POINT('',(152.5,-125.,47.));
#19212=CARTESIAN_POINT('Origin',(147.5,-125.,44.5));
#19213=CARTESIAN_POINT('Origin',(0.,0.,-105.));
#19214=CARTESIAN_POINT('Origin',(-115.,0.,-105.));
#19215=CARTESIAN_POINT('',(-96.695242233189,174.040040919032,-44.9999999999999));
#19216=CARTESIAN_POINT('Origin',(-115.,0.,-44.9999999999999));
#19217=CARTESIAN_POINT('',(-96.695242233189,174.040040919032,45.0000000000001));
#19218=CARTESIAN_POINT('Origin',(-115.,0.,45.0000000000001));
#19219=CARTESIAN_POINT('',(-96.695242233189,174.040040919032,-105.));
#19220=CARTESIAN_POINT('Origin',(-115.000000000001,175.,80.0000000000001));
#19221=CARTESIAN_POINT('',(-93.0342906798268,208.848049102839,80.0000000000001));
#19222=CARTESIAN_POINT('',(-14.5652173913043,184.425742352699,80.));
#19223=CARTESIAN_POINT('Origin',(-115.,0.,80.0000000000001));
#19224=CARTESIAN_POINT('',(65.4347826086958,173.041293409847,80.));
#19225=CARTESIAN_POINT('Origin',(-3.78485122031303E-15,0.,80.));
#19226=CARTESIAN_POINT('',(-108.033967922038,249.902929948988,80.0000000000001));
#19227=CARTESIAN_POINT('Origin',(-115.,0.,80.0000000000001));
#19228=CARTESIAN_POINT('',(-108.033967922038,209.585728186396,80.0000000000001));
#19229=CARTESIAN_POINT('',(-108.033967922038,175.,80.0000000000001));
#19230=CARTESIAN_POINT('Origin',(-107.155103814224,74.5885889652995,80.0000000000001));
#19231=CARTESIAN_POINT('Origin',(-115.,0.,-105.));
#19232=CARTESIAN_POINT('',(-107.058723431124,284.889340141846,-44.9999999999999));
#19233=CARTESIAN_POINT('Origin',(-115.,0.,-44.9999999999999));
#19234=CARTESIAN_POINT('',(-115.000000000001,285.,-45.1798442476466));
#19235=CARTESIAN_POINT('Origin',(-109.23990359688,206.681571026642,-172.26199221829));
#19236=CARTESIAN_POINT('',(-115.000000000001,285.,45.1798442476468));
#19237=CARTESIAN_POINT('',(-115.000000000001,285.,2.44375389117379E-28));
#19238=CARTESIAN_POINT('',(-107.058723431124,284.889340141846,45.0000000000001));
#19239=CARTESIAN_POINT('Origin',(-109.239903596884,206.681571026862,172.261992218181));
#19240=CARTESIAN_POINT('Origin',(-115.,0.,45.0000000000001));
#19241=CARTESIAN_POINT('Origin',(-115.000000000001,175.,-79.9999999999999));
#19242=CARTESIAN_POINT('',(-108.033967922038,249.902929948988,-79.9999999999999));
#19243=CARTESIAN_POINT('',(65.4347826086956,173.041293409847,-80.));
#19244=CARTESIAN_POINT('Origin',(-115.,0.,-79.9999999999999));
#19245=CARTESIAN_POINT('',(-14.5652173913044,184.425742352699,-80.));
#19246=CARTESIAN_POINT('Origin',(3.78485122031304E-15,0.,-80.));
#19247=CARTESIAN_POINT('',(-93.0342906798268,208.848049102839,-79.9999999999999));
#19248=CARTESIAN_POINT('Origin',(-115.,0.,-79.9999999999999));
#19249=CARTESIAN_POINT('',(-108.033967922038,209.585728186396,-79.9999999999999));
#19250=CARTESIAN_POINT('Origin',(-107.155103814224,74.5885889652995,-79.9999999999999));
#19251=CARTESIAN_POINT('',(-108.033967922039,285.,-79.9999999999999));
#19252=CARTESIAN_POINT('Origin',(-365.,-1.26634813746307E-12,8.80937834756918E-14));
#19253=CARTESIAN_POINT('',(-365.000000000001,249.999999999999,-115.));
#19254=CARTESIAN_POINT('',(-365.000000000001,159.722601683408,-115.));
#19255=CARTESIAN_POINT('',(-365.000000000001,284.999999999999,-115.));
#19256=CARTESIAN_POINT('',(-365.000000000001,124.999999999999,-80.6196334903569));
#19257=CARTESIAN_POINT('Origin',(-365.000000000001,160.693136595148,-79.658664428181));
#19258=CARTESIAN_POINT('',(-365.000000000001,124.999999999999,80.6196334903571));
#19259=CARTESIAN_POINT('',(-365.000000000001,124.999999999999,-115.));
#19260=CARTESIAN_POINT('',(-365.000000000001,159.722601683408,115.));
#19261=CARTESIAN_POINT('Origin',(-365.000000000001,160.693136595149,79.6586644281792));
#19262=CARTESIAN_POINT('',(-365.000000000001,249.999999999999,115.));
#19263=CARTESIAN_POINT('',(-365.000000000001,284.999999999999,115.));
#19264=CARTESIAN_POINT('',(-365.000000000001,284.999999999999,79.65866442818));
#19265=CARTESIAN_POINT('Origin',(-365.000000000001,249.999999999999,79.6586644281791));
#19266=CARTESIAN_POINT('',(-365.000000000001,284.999999999999,-79.6586644281798));
#19267=CARTESIAN_POINT('',(-365.000000000001,284.999999999999,-115.));
#19268=CARTESIAN_POINT('Origin',(-365.000000000001,250.,-79.6586644281799));
#19269=CARTESIAN_POINT('',(-365.000000000001,249.999999999999,-104.902475550908));
#19270=CARTESIAN_POINT('',(-365.000000000001,159.999897372477,-104.902475550908));
#19271=CARTESIAN_POINT('',(-365.,-1.26634813746307E-12,-104.902475550908));
#19272=CARTESIAN_POINT('',(-365.000000000001,274.999999999999,-79.6586644281798));
#19273=CARTESIAN_POINT('Origin',(-365.000000000001,249.999999999997,-79.6586644281774));
#19274=CARTESIAN_POINT('',(-365.000000000001,274.999999999999,79.65866442818));
#19275=CARTESIAN_POINT('',(-365.000000000001,274.999999999999,8.8093783475692E-14));
#19276=CARTESIAN_POINT('',(-365.000000000001,250.,104.902475550909));
#19277=CARTESIAN_POINT('Origin',(-365.000000000001,249.999999999998,79.6586644281787));
#19278=CARTESIAN_POINT('',(-365.000000000001,159.999897372477,104.902475550909));
#19279=CARTESIAN_POINT('',(-365.,-1.26634813746307E-12,104.902475550909));
#19280=CARTESIAN_POINT('',(-365.000000000001,135.198039027185,80.3450709011636));
#19281=CARTESIAN_POINT('Origin',(-365.000000000001,160.693136595147,79.6586644281815));
#19282=CARTESIAN_POINT('',(-365.000000000001,135.198039027185,-80.3450709011634));
#19283=CARTESIAN_POINT('',(-365.000000000001,135.198039027185,8.80937834756919E-14));
#19284=CARTESIAN_POINT('Origin',(-365.,160.693136595149,-79.6586644281788));
#19285=CARTESIAN_POINT('Origin',(-1.01252339845814E-12,285.,2.44375389117379E-28));
#19286=CARTESIAN_POINT('',(-126.751426934183,285.,-46.3038641989653));
#19287=CARTESIAN_POINT('Origin',(-108.033967922039,285.,-180.));
#19288=CARTESIAN_POINT('',(3.92135447228731,285.,-28.0096748020595));
#19289=CARTESIAN_POINT('',(-126.751426934183,285.,46.3038641989655));
#19290=CARTESIAN_POINT('',(3.92135447228733,285.,28.0096748020595));
#19291=CARTESIAN_POINT('Origin',(-108.033967922038,285.,180.));
#19292=CARTESIAN_POINT('Origin',(8.77402903099257,3.04410282779297E-14,
62.6716359356611));
#19293=CARTESIAN_POINT('',(-128.778107499175,206.966980183574,81.9289350498845));
#19294=CARTESIAN_POINT('',(-35.4836922769749,225.625863228014,68.8677169187765));
#19295=CARTESIAN_POINT('',(-121.898752375479,208.15873578029,80.965825332567));
#19296=CARTESIAN_POINT('Origin',(-102.313983178497,72.0502950009906,78.2239576449902));
#19297=CARTESIAN_POINT('',(-121.898752375479,250.,80.965825332567));
#19298=CARTESIAN_POINT('',(-121.898752375479,285.,80.965825332567));
#19299=CARTESIAN_POINT('',(8.77402903099168,250.,62.6716359356611));
#19300=CARTESIAN_POINT('Origin',(8.77402903099253,3.04410282779296E-14,
-62.671635935661));
#19301=CARTESIAN_POINT('',(-121.898752375479,250.,-80.9658253325669));
#19302=CARTESIAN_POINT('',(-121.898752375479,208.15873578029,-80.9658253325669));
#19303=CARTESIAN_POINT('',(-121.898752375479,175.,-80.9658253325669));
#19304=CARTESIAN_POINT('',(-128.778107499175,206.966980183574,-81.9289350498844));
#19305=CARTESIAN_POINT('Origin',(-102.313983154048,72.050294857119,-78.2239576415826));
#19306=CARTESIAN_POINT('',(-35.4836922769749,225.625863228014,-68.8677169187764));
#19307=CARTESIAN_POINT('',(8.77402903099165,250.,-62.671635935661));
#19308=CARTESIAN_POINT('Origin',(-38.0769230769238,190.384615384616,9.1899731971482E-15));
#19309=CARTESIAN_POINT('',(-126.766717328043,172.646656534391,-47.2669739162828));
#19310=CARTESIAN_POINT('',(-33.4723021058426,191.305539578832,-34.2057557851748));
#19311=CARTESIAN_POINT('',(-126.766717328043,172.646656534391,47.2669739162829));
#19312=CARTESIAN_POINT('',(-126.766717328043,172.646656534391,80.));
#19313=CARTESIAN_POINT('',(-33.4723021058425,191.305539578832,34.2057557851749));
#19314=CARTESIAN_POINT('Origin',(-108.033967922037,-3.74818120714568E-13,
180.));
#19315=CARTESIAN_POINT('Ctrl Pts',(-121.898752375479,208.15873578029,80.965825332567));
#19316=CARTESIAN_POINT('Ctrl Pts',(-119.963682399492,208.541997665569,80.6949155359288));
#19317=CARTESIAN_POINT('Ctrl Pts',(-118.016904254303,208.849389003878,80.4801212165123));
#19318=CARTESIAN_POINT('Ctrl Pts',(-116.058201668433,209.079632070727,80.3224566800619));
#19319=CARTESIAN_POINT('Ctrl Pts',(-115.706309545742,209.120996554602,80.294131344299));
#19320=CARTESIAN_POINT('Ctrl Pts',(-115.35403253681,209.159870880317,80.2676500224512));
#19321=CARTESIAN_POINT('Ctrl Pts',(-115.001369373232,209.19624749802,80.2430187053663));
#19322=CARTESIAN_POINT('Ctrl Pts',(-113.243049246847,209.37761528928,80.12021103776));
#19323=CARTESIAN_POINT('Ctrl Pts',(-111.475122526152,209.496902484032,80.0433849490804));
#19324=CARTESIAN_POINT('Ctrl Pts',(-109.697347830952,209.55244226832,80.0138248285002));
#19325=CARTESIAN_POINT('Ctrl Pts',(-109.143844976527,209.569734352194,80.004621406288));
#19326=CARTESIAN_POINT('Ctrl Pts',(-108.589387464291,209.580846699948,80.0000000000001));
#19327=CARTESIAN_POINT('Ctrl Pts',(-108.033967922038,209.585728186396,80.0000000000001));
#19328=CARTESIAN_POINT('',(-113.193991683492,250.,80.1332179612198));
#19329=CARTESIAN_POINT('Origin',(-109.82357655303,202.360240296963,145.359472475069));
#19330=CARTESIAN_POINT('Origin',(-108.033967922038,250.,180.));
#19331=CARTESIAN_POINT('Origin',(-107.155103814224,74.5885889652995,-105.));
#19332=CARTESIAN_POINT('',(-121.670898717897,173.529438457885,-46.3038641989653));
#19333=CARTESIAN_POINT('',(-107.806114264457,174.586469869815,-44.9999999999999));
#19334=CARTESIAN_POINT('Ctrl Pts',(-121.670898717897,173.529438457885,-46.3038641989653));
#19335=CARTESIAN_POINT('Ctrl Pts',(-119.700296307634,173.818549179804,-45.9314203435801));
#19336=CARTESIAN_POINT('Ctrl Pts',(-117.717862072481,174.049330964995,-45.6375988479542));
#19337=CARTESIAN_POINT('Ctrl Pts',(-115.723382153899,174.220839876011,-45.4237707689551));
#19338=CARTESIAN_POINT('Ctrl Pts',(-115.407063289645,174.248040703373,-45.3898582414514));
#19339=CARTESIAN_POINT('Ctrl Pts',(-115.090441431131,174.273750575165,-45.3579578799593));
#19340=CARTESIAN_POINT('Ctrl Pts',(-114.773515715655,174.297965656261,-45.3280752522696));
#19341=CARTESIAN_POINT('Ctrl Pts',(-112.980668894128,174.434950220962,-45.1590294113797));
#19342=CARTESIAN_POINT('Ctrl Pts',(-111.178090500797,174.524105770559,-45.0545447965882));
#19343=CARTESIAN_POINT('Ctrl Pts',(-109.365535898701,174.564165311637,-45.0164029276363));
#19344=CARTESIAN_POINT('Ctrl Pts',(-108.846548544408,174.575635528984,-45.0054817958634));
#19345=CARTESIAN_POINT('Ctrl Pts',(-108.326743269188,174.583080448762,-44.9999999999999));
#19346=CARTESIAN_POINT('Ctrl Pts',(-107.806114264457,174.586469869815,-44.9999999999999));
#19347=CARTESIAN_POINT('Origin',(-107.155103814224,74.5885889652995,-44.9999999999999));
#19348=CARTESIAN_POINT('',(-107.806114264457,174.586469869815,45.0000000000001));
#19349=CARTESIAN_POINT('Origin',(-107.155103814224,74.5885889652995,45.0000000000001));
#19350=CARTESIAN_POINT('',(-121.670898717897,173.529438457885,46.3038641989655));
#19351=CARTESIAN_POINT('Ctrl Pts',(-107.806114264457,174.586469869815,45.));
#19352=CARTESIAN_POINT('Ctrl Pts',(-109.624402314666,174.574632373745,45.));
#19353=CARTESIAN_POINT('Ctrl Pts',(-111.432643308778,174.51333051059,45.0668606225803));
#19354=CARTESIAN_POINT('Ctrl Pts',(-113.231083127889,174.403839947209,45.1987882647131));
#19355=CARTESIAN_POINT('Ctrl Pts',(-113.74602899258,174.37248959996,45.2365630031463));
#19356=CARTESIAN_POINT('Ctrl Pts',(-114.260171286305,174.337188339623,45.2796724887734));
#19357=CARTESIAN_POINT('Ctrl Pts',(-114.773515715654,174.297965656261,45.3280752522816));
#19358=CARTESIAN_POINT('Ctrl Pts',(-116.77182207048,174.145282714882,45.5164936793255));
#19359=CARTESIAN_POINT('Ctrl Pts',(-118.758048443814,173.933174431027,45.785126873589));
#19360=CARTESIAN_POINT('Ctrl Pts',(-120.732409349687,173.662589501794,46.1325970502785));
#19361=CARTESIAN_POINT('Ctrl Pts',(-121.045537318146,173.619675509253,46.1877048222179));
#19362=CARTESIAN_POINT('Ctrl Pts',(-121.358366825477,173.575290589482,46.2447956712981));
#19363=CARTESIAN_POINT('Ctrl Pts',(-121.670898717897,173.529438457885,46.3038641989655));
#19364=CARTESIAN_POINT('Origin',(-107.172158244333,71.1720523181789,43.5636022494356));
#19365=CARTESIAN_POINT('Origin',(-107.172158244267,71.1720523177554,-43.5636022494229));
#19366=CARTESIAN_POINT('Origin',(-108.033967922038,-3.74818120714567E-13,
-180.));
#19367=CARTESIAN_POINT('Ctrl Pts',(-108.033967922038,209.585728186396,-79.9999999999999));
#19368=CARTESIAN_POINT('Ctrl Pts',(-109.817898725999,209.570049526606,-79.9999999999999));
#19369=CARTESIAN_POINT('Ctrl Pts',(-111.591905506614,209.490096075732,-80.0476722982013));
#19370=CARTESIAN_POINT('Ctrl Pts',(-113.356231010759,209.347547495565,-80.1417226834948));
#19371=CARTESIAN_POINT('Ctrl Pts',(-113.905546550713,209.303165577319,-80.1710048868405));
#19372=CARTESIAN_POINT('Ctrl Pts',(-114.453923591632,209.252715618219,-80.204783040216));
#19373=CARTESIAN_POINT('Ctrl Pts',(-115.001369373232,209.19624749802,-80.2430187053662));
#19374=CARTESIAN_POINT('Ctrl Pts',(-116.964363679643,208.993767906125,-80.3801215848005));
#19375=CARTESIAN_POINT('Ctrl Pts',(-118.915394248576,208.713906143843,-80.574539846874));
#19376=CARTESIAN_POINT('Ctrl Pts',(-120.85467810225,208.357947311172,-80.8252534637792));
#19377=CARTESIAN_POINT('Ctrl Pts',(-121.203081595339,208.293997260506,-80.8702956063874));
#19378=CARTESIAN_POINT('Ctrl Pts',(-121.551105938358,208.227590979612,-80.9171548313701));
#19379=CARTESIAN_POINT('Ctrl Pts',(-121.898752375479,208.15873578029,-80.9658253325669));
#19380=CARTESIAN_POINT('',(-113.193991683492,250.,-80.1332179612197));
#19381=CARTESIAN_POINT('Origin',(-108.033967922038,250.,-180.));
#19382=CARTESIAN_POINT('Origin',(-109.823576553026,202.360240296967,-145.359472475138));
#19383=CARTESIAN_POINT('Origin',(-40.3363668356791,225.625863228014,-34.2057557851748));
#19384=CARTESIAN_POINT('Origin',(-133.630782057879,206.966980183574,-47.2669739162828));
#19385=CARTESIAN_POINT('Ctrl Pts',(-121.670898717897,173.529438457885,-46.3038641989654));
#19386=CARTESIAN_POINT('Ctrl Pts',(-117.014194117273,174.212632196936,-80.2819871764181));
#19387=CARTESIAN_POINT('Ctrl Pts',(-121.898752375479,208.15873578029,-80.9658253325669));
#19388=CARTESIAN_POINT('Ctrl Pts',(-123.376736606944,173.279171828244,-46.6262675599635));
#19389=CARTESIAN_POINT('Ctrl Pts',(-118.752370779928,174.039540392877,-80.5253319092667));
#19390=CARTESIAN_POINT('Ctrl Pts',(-124.201633525808,207.820875830255,-81.288228693613));
#19391=CARTESIAN_POINT('Ctrl Pts',(-125.076099494733,172.984780101053,-46.9474471457602));
#19392=CARTESIAN_POINT('Ctrl Pts',(-120.48990998314,173.820474755941,-80.7685873976411));
#19393=CARTESIAN_POINT('Ctrl Pts',(-126.495773409627,207.423447001444,-81.6094082773477));
#19394=CARTESIAN_POINT('Ctrl Pts',(-126.766717328043,172.646656534391,-47.2669739162828));
#19395=CARTESIAN_POINT('Ctrl Pts',(-122.224200046663,173.555159990667,-81.0113880065327));
#19396=CARTESIAN_POINT('Ctrl Pts',(-128.778107499175,206.966980183574,-81.9289350498844));
#19397=CARTESIAN_POINT('Origin',(-126.751426934183,208.15873578029,-46.3038641989653));
#19398=CARTESIAN_POINT('Ctrl Pts',(-107.806114264457,174.586469869815,-44.9999999999999));
#19399=CARTESIAN_POINT('Ctrl Pts',(-107.806114264457,174.586469869815,-79.9999999999999));
#19400=CARTESIAN_POINT('Ctrl Pts',(-108.033967922038,209.585728186396,-79.9999999999999));
#19401=CARTESIAN_POINT('Ctrl Pts',(-110.140392035471,174.571273155555,-44.9999999999671));
#19402=CARTESIAN_POINT('Ctrl Pts',(-109.323233110512,174.576593058387,-79.9946819508194));
#19403=CARTESIAN_POINT('Ctrl Pts',(-110.368245901835,209.565212620414,-79.9999999999999));
#19404=CARTESIAN_POINT('Ctrl Pts',(-112.462776734628,174.47452037898,-45.1101978466298));
#19405=CARTESIAN_POINT('Ctrl Pts',(-110.831769330981,174.542829711498,-80.0133399190488));
#19406=CARTESIAN_POINT('Ctrl Pts',(-112.690630392213,209.434596373781,-80.0816280345504));
#19407=CARTESIAN_POINT('Ctrl Pts',(-117.084254696684,174.121410933542,-45.5459526578601));
#19408=CARTESIAN_POINT('Ctrl Pts',(-113.886869252213,174.421832152824,-80.1038421118365));
#19409=CARTESIAN_POINT('Ctrl Pts',(-117.312108354263,208.957898622415,-80.4044093761828));
#19410=CARTESIAN_POINT('Ctrl Pts',(-119.383361285263,173.865047302734,-45.8715196243769));
#19411=CARTESIAN_POINT('Ctrl Pts',(-115.428565673966,174.334921360029,-80.1754126412373));
#19412=CARTESIAN_POINT('Ctrl Pts',(-119.611215134969,208.611807682755,-80.6455701188955));
#19413=CARTESIAN_POINT('Ctrl Pts',(-121.670898717897,173.529438457885,-46.3038641989653));
#19414=CARTESIAN_POINT('Ctrl Pts',(-117.014194117273,174.212632196936,-80.2819871764181));
#19415=CARTESIAN_POINT('Ctrl Pts',(-121.898752375479,208.15873578029,-80.9658253325669));
#19416=CARTESIAN_POINT('Origin',(-108.033967922038,209.585728186396,-44.9999999999999));
#19417=CARTESIAN_POINT('Origin',(-107.155103814224,74.5885889652995,-44.9999999999999));
#19418=CARTESIAN_POINT('Origin',(-93.0342906798268,208.848049102839,-44.9999999999999));
#19419=CARTESIAN_POINT('Origin',(-115.,0.,-44.9999999999999));
#19420=CARTESIAN_POINT('Ctrl Pts',(-14.5652173913044,184.425742352699,-80.));
#19421=CARTESIAN_POINT('Ctrl Pts',(-16.5344677033485,184.565305142146,-80.));
#19422=CARTESIAN_POINT('Ctrl Pts',(-18.5002973477175,184.673702607589,-79.9714170458664));
#19423=CARTESIAN_POINT('Ctrl Pts',(-20.462612886933,184.751448877997,-79.9131822068492));
#19424=CARTESIAN_POINT('Ctrl Pts',(-22.3952938122587,184.82802103514,-79.8558268221983));
#19425=CARTESIAN_POINT('Ctrl Pts',(-24.324565992262,184.87486103494,-79.7697082616294));
#19426=CARTESIAN_POINT('Ctrl Pts',(-26.2503475316718,184.892497907978,-79.6538362317921));
#19427=CARTESIAN_POINT('Ctrl Pts',(-26.5018085199062,184.894800861575,-79.6387061173241));
#19428=CARTESIAN_POINT('Ctrl Pts',(-26.7532096955271,184.896605367196,-79.6230686927859));
#19429=CARTESIAN_POINT('Ctrl Pts',(-27.0045509729748,184.897912683916,-79.6069217821172));
#19430=CARTESIAN_POINT('Ctrl Pts',(-28.9907477845154,184.90824361057,-79.4793225958153));
#19431=CARTESIAN_POINT('Ctrl Pts',(-30.9732260056195,184.887510891604,-79.319970845809));
#19432=CARTESIAN_POINT('Ctrl Pts',(-32.951755848961,184.836136694374,-79.1264843643942));
#19433=CARTESIAN_POINT('Ctrl Pts',(-34.58712483348,184.793672958465,-78.966556632349));
#19434=CARTESIAN_POINT('Ctrl Pts',(-36.2197964305512,184.730275751757,-78.78330862021));
#19435=CARTESIAN_POINT('Ctrl Pts',(-37.8496463618853,184.646200267918,-78.5754154614948));
#19436=CARTESIAN_POINT('Ctrl Pts',(-38.3445529765253,184.620670608848,-78.512288361626));
#19437=CARTESIAN_POINT('Ctrl Pts',(-38.8391670257304,184.59323304001,-78.4468923527209));
#19438=CARTESIAN_POINT('Ctrl Pts',(-39.3334992489681,184.563894543215,-78.3791893119185));
#19439=CARTESIAN_POINT('Ctrl Pts',(-40.9140488305578,184.470089311321,-78.1627194809377));
#19440=CARTESIAN_POINT('Ctrl Pts',(-42.4916983624513,184.356837819108,-77.9225453086862));
#19441=CARTESIAN_POINT('Ctrl Pts',(-44.0666753706419,184.224296659025,-77.6566322107026));
#19442=CARTESIAN_POINT('Ctrl Pts',(-44.5304989103894,184.18526389238,-77.5783220171376));
#19443=CARTESIAN_POINT('Ctrl Pts',(-44.9940906480806,184.144557963664,-77.4977792877235));
#19444=CARTESIAN_POINT('Ctrl Pts',(-45.4574563428166,184.102182331615,-77.4149513693389));
#19445=CARTESIAN_POINT('Ctrl Pts',(-46.4756789541978,184.00906402956,-77.2329412198805));
#19446=CARTESIAN_POINT('Ctrl Pts',(-47.4928067767693,183.907882722016,-77.0398762547174));
#19447=CARTESIAN_POINT('Ctrl Pts',(-48.5088764533298,183.798668678686,-76.8350434911382));
#19448=CARTESIAN_POINT('Ctrl Pts',(-48.7905784132376,183.768389446105,-76.7782542843696));
#19449=CARTESIAN_POINT('Ctrl Pts',(-49.072205880457,183.73748883725,-76.7205542596092));
#19450=CARTESIAN_POINT('Ctrl Pts',(-49.353594996623,183.705990252679,-76.6619665200221));
#19451=CARTESIAN_POINT('Ctrl Pts',(-50.0860997232609,183.623993967981,-76.509452461357));
#19452=CARTESIAN_POINT('Ctrl Pts',(-50.817661700711,183.537867720617,-76.3507823667154));
#19453=CARTESIAN_POINT('Ctrl Pts',(-51.5454344349616,183.447993539071,-76.1863137058566));
#19454=CARTESIAN_POINT('Ctrl Pts',(-52.5893488086163,183.319078363329,-75.9504004997055));
#19455=CARTESIAN_POINT('Ctrl Pts',(-53.6275144052881,183.182241566705,-75.7021915460668));
#19456=CARTESIAN_POINT('Ctrl Pts',(-54.6599414688518,183.0377363009,-75.4409038988655));
#19457=CARTESIAN_POINT('Ctrl Pts',(-55.6097700716653,182.904792057609,-75.2005203505914));
#19458=CARTESIAN_POINT('Ctrl Pts',(-56.5547414352707,182.765357070629,-74.9490668063843));
#19459=CARTESIAN_POINT('Ctrl Pts',(-57.4948450401202,182.619621548287,-74.6858999615784));
#19460=CARTESIAN_POINT('Ctrl Pts',(-58.4547719007016,182.470813010893,-74.4171839159847));
#19461=CARTESIAN_POINT('Ctrl Pts',(-59.4096299264397,182.315431591912,-74.136266643455));
#19462=CARTESIAN_POINT('Ctrl Pts',(-60.3592589587275,182.153712006982,-73.8422126425771));
#19463=CARTESIAN_POINT('Ctrl Pts',(-60.4364200749712,182.140571650835,-73.8183195915306));
#19464=CARTESIAN_POINT('Ctrl Pts',(-60.5135466547183,182.127389446893,-73.7943397839875));
#19465=CARTESIAN_POINT('Ctrl Pts',(-60.5906386047577,182.114165520119,-73.7702727046069));
#19466=CARTESIAN_POINT('Ctrl Pts',(-61.4871617108446,181.960380904474,-73.4903901390501));
#19467=CARTESIAN_POINT('Ctrl Pts',(-62.378843094726,181.800977623905,-73.1987553513707));
#19468=CARTESIAN_POINT('Ctrl Pts',(-63.2654994241718,181.636164462385,-72.8945617944821));
#19469=CARTESIAN_POINT('Ctrl Pts',(-64.1932340557345,181.463715597361,-72.5762751167111));
#19470=CARTESIAN_POINT('Ctrl Pts',(-65.1154789896928,181.285337902937,-72.2442595652156));
#19471=CARTESIAN_POINT('Ctrl Pts',(-66.0318123592137,181.101342645502,-71.8972293164849));
#19472=CARTESIAN_POINT('Ctrl Pts',(-66.8326026625298,180.940547870466,-71.5939570933133));
#19473=CARTESIAN_POINT('Ctrl Pts',(-67.6288742820847,180.775468201812,-71.2792231566612));
#19474=CARTESIAN_POINT('Ctrl Pts',(-68.4204040726826,180.606290606281,-70.9520943939504));
#19475=CARTESIAN_POINT('Ctrl Pts',(-68.5608266260415,180.576277396143,-70.8940596153702));
#19476=CARTESIAN_POINT('Ctrl Pts',(-68.7010998749578,180.546135213193,-70.835634617901));
#19477=CARTESIAN_POINT('Ctrl Pts',(-68.841222488813,180.515865104335,-70.7768140396236));
#19478=CARTESIAN_POINT('Ctrl Pts',(-69.5818936550052,180.355860975009,-70.4658955867758));
#19479=CARTESIAN_POINT('Ctrl Pts',(-70.3183392970407,180.192289767342,-70.1438963096542));
#19480=CARTESIAN_POINT('Ctrl Pts',(-71.050229845743,180.025357594668,-69.8097965221065));
#19481=CARTESIAN_POINT('Ctrl Pts',(-71.1460330992753,180.003506451366,-69.7660634165099));
#19482=CARTESIAN_POINT('Ctrl Pts',(-71.2417582683773,179.981597725142,-69.7221229124221));
#19483=CARTESIAN_POINT('Ctrl Pts',(-71.3374045811306,179.959631883187,-69.6779726643808));
#19484=CARTESIAN_POINT('Ctrl Pts',(-71.407777809868,179.943470181017,-69.6454884481597));
#19485=CARTESIAN_POINT('Ctrl Pts',(-71.4781084628288,179.927277560157,-69.612890661583));
#19486=CARTESIAN_POINT('Ctrl Pts',(-71.5483972204143,179.911053977661,-69.5801779008149));
#19487=CARTESIAN_POINT('Ctrl Pts',(-71.9837167618859,179.810576422841,-69.3775778761874));
#19488=CARTESIAN_POINT('Ctrl Pts',(-72.4175547523421,179.708871552097,-69.1704715579982));
#19489=CARTESIAN_POINT('Ctrl Pts',(-72.8489072435447,179.606229298099,-68.9591086722214));
#19490=CARTESIAN_POINT('Ctrl Pts',(-73.2108088745924,179.520113186812,-68.7817767345008));
#19491=CARTESIAN_POINT('Ctrl Pts',(-73.5709606302885,179.433337187436,-68.601448242336));
#19492=CARTESIAN_POINT('Ctrl Pts',(-73.9287415278322,179.346076081554,-68.4182667355679));
#19493=CARTESIAN_POINT('Ctrl Pts',(-74.0152614109623,179.324974282283,-68.3739691146888));
#19494=CARTESIAN_POINT('Ctrl Pts',(-74.1016508240775,179.303841974661,-68.329500240179));
#19495=CARTESIAN_POINT('Ctrl Pts',(-74.1878981569291,179.282682307813,-68.2848633631352));
#19496=CARTESIAN_POINT('Ctrl Pts',(-74.9520405519443,179.095209861207,-67.8893852770014));
#19497=CARTESIAN_POINT('Ctrl Pts',(-75.7068985668535,178.905157510695,-67.4799676364347));
#19498=CARTESIAN_POINT('Ctrl Pts',(-76.4510161725052,178.71327515797,-67.0555357540613));
#19499=CARTESIAN_POINT('Ctrl Pts',(-76.9578846194199,178.582571208248,-66.7664267108056));
#19500=CARTESIAN_POINT('Ctrl Pts',(-77.4598402991781,178.450997227197,-66.4703085533318));
#19501=CARTESIAN_POINT('Ctrl Pts',(-77.9566463445384,178.318729280589,-66.1666611079086));
#19502=CARTESIAN_POINT('Ctrl Pts',(-78.3570807339144,178.212118994889,-65.921915939187));
#19503=CARTESIAN_POINT('Ctrl Pts',(-78.7541689603514,178.105058023274,-65.6722787015837));
#19504=CARTESIAN_POINT('Ctrl Pts',(-79.1477690647678,177.997644212194,-65.4174609479341));
#19505=CARTESIAN_POINT('Ctrl Pts',(-79.5939502217359,177.875880986106,-65.1286020811207));
#19506=CARTESIAN_POINT('Ctrl Pts',(-80.03566857104,177.753656057224,-64.833103516267));
#19507=CARTESIAN_POINT('Ctrl Pts',(-80.4725490551237,177.63117690159,-64.5303986499002));
#19508=CARTESIAN_POINT('Ctrl Pts',(-80.7344890850065,177.557742186936,-64.3489061716813));
#19509=CARTESIAN_POINT('Ctrl Pts',(-80.9946892979568,177.48421632754,-64.1648225373259));
#19510=CARTESIAN_POINT('Ctrl Pts',(-81.2530623554429,177.410646455889,-63.9780198133583));
#19511=CARTESIAN_POINT('Ctrl Pts',(-81.6419444022845,177.299915087256,-63.696859593485));
#19512=CARTESIAN_POINT('Ctrl Pts',(-82.0267334585135,177.189095393788,-63.4095470563223));
#19513=CARTESIAN_POINT('Ctrl Pts',(-82.4071387809341,177.078326593046,-63.1155673632256));
#19514=CARTESIAN_POINT('Ctrl Pts',(-82.7804815138832,176.969614321275,-62.8270456849435));
#19515=CARTESIAN_POINT('Ctrl Pts',(-83.1496018524829,176.860950988961,-62.5321021503129));
#19516=CARTESIAN_POINT('Ctrl Pts',(-83.5141887379417,176.752482541153,-62.2302206105805));
#19517=CARTESIAN_POINT('Ctrl Pts',(-83.5514766168838,176.741389003475,-62.1993458787748));
#19518=CARTESIAN_POINT('Ctrl Pts',(-83.5887172775307,176.730297571654,-62.1683985707106));
#19519=CARTESIAN_POINT('Ctrl Pts',(-83.6259104466999,176.719208410275,-62.1373780905463));
#19520=CARTESIAN_POINT('Ctrl Pts',(-83.9558178441684,176.620846360133,-61.8622231062355));
#19521=CARTESIAN_POINT('Ctrl Pts',(-84.2819553798721,176.522676464612,-61.5812821073024));
#19522=CARTESIAN_POINT('Ctrl Pts',(-84.604034142111,176.424851647322,-61.2940527224133));
#19523=CARTESIAN_POINT('Ctrl Pts',(-84.6228412574001,176.41913937184,-61.2772805635833));
#19524=CARTESIAN_POINT('Ctrl Pts',(-84.6416345369846,176.413428270688,-61.260486939101));
#19525=CARTESIAN_POINT('Ctrl Pts',(-84.6604139206614,176.407718374571,-61.2436717431479));
#19526=CARTESIAN_POINT('Ctrl Pts',(-84.8808984780687,176.340679757123,-61.0462482759436));
#19527=CARTESIAN_POINT('Ctrl Pts',(-85.0996941313493,176.273736013823,-60.8456211532969));
#19528=CARTESIAN_POINT('Ctrl Pts',(-85.3158922454133,176.207191546391,-60.6423925159304));
#19529=CARTESIAN_POINT('Ctrl Pts',(-85.4300515625353,176.172054001399,-60.5350814852035));
#19530=CARTESIAN_POINT('Ctrl Pts',(-85.5434859458774,176.137028005454,-60.4270455100516));
#19531=CARTESIAN_POINT('Ctrl Pts',(-85.6560566970487,176.102159964998,-60.3183761224715));
#19532=CARTESIAN_POINT('Ctrl Pts',(-85.6581590166629,176.101508785499,-60.3163466629308));
#19533=CARTESIAN_POINT('Ctrl Pts',(-85.6602610537763,176.100857655553,-60.3143169678148));
#19534=CARTESIAN_POINT('Ctrl Pts',(-85.6623628082838,176.100206575221,-60.3122870370121));
#19535=CARTESIAN_POINT('Ctrl Pts',(-85.9655775819481,176.006276872874,-60.0194340864486));
#19536=CARTESIAN_POINT('Ctrl Pts',(-86.2628725546031,175.913391296893,-59.7217178015255));
#19537=CARTESIAN_POINT('Ctrl Pts',(-86.5539294847292,175.821739230135,-59.4187834172871));
#19538=CARTESIAN_POINT('Ctrl Pts',(-86.839402798911,175.731845410264,-59.1216605052483));
#19539=CARTESIAN_POINT('Ctrl Pts',(-87.1188751736362,175.643138147991,-58.8195178119657));
#19540=CARTESIAN_POINT('Ctrl Pts',(-87.3920035701138,175.555813880903,-58.5120004904891));
#19541=CARTESIAN_POINT('Ctrl Pts',(-87.426799101105,175.544689097538,-58.4728239397248));
#19542=CARTESIAN_POINT('Ctrl Pts',(-87.4614916119104,175.533586784895,-58.4335601321732));
#19543=CARTESIAN_POINT('Ctrl Pts',(-87.4960803413495,175.522507371371,-58.3942083096898));
#19544=CARTESIAN_POINT('Ctrl Pts',(-87.7552552800019,175.439488816853,-58.0993432960449));
#19545=CARTESIAN_POINT('Ctrl Pts',(-88.0086095980277,175.357753517098,-57.7995395611124));
#19546=CARTESIAN_POINT('Ctrl Pts',(-88.25573352756,175.277510566065,-57.4944372405943));
#19547=CARTESIAN_POINT('Ctrl Pts',(-88.4979680292567,175.198855248083,-57.1953714693554));
#19548=CARTESIAN_POINT('Ctrl Pts',(-88.734216305342,175.12163374876,-56.8912147377849));
#19549=CARTESIAN_POINT('Ctrl Pts',(-88.9640500525986,175.046061324727,-56.5816081863863));
#19550=CARTESIAN_POINT('Ctrl Pts',(-89.0160581643391,175.028960358831,-56.5115486224061));
#19551=CARTESIAN_POINT('Ctrl Pts',(-89.067737641556,175.011943911971,-56.4412099156939));
#19552=CARTESIAN_POINT('Ctrl Pts',(-89.1190832067734,174.995014617266,-56.370587759921));
#19553=CARTESIAN_POINT('Ctrl Pts',(-89.2169920966178,174.962732794223,-56.2359210785657));
#19554=CARTESIAN_POINT('Ctrl Pts',(-89.3136877484593,174.930767566929,-56.1002241654811));
#19555=CARTESIAN_POINT('Ctrl Pts',(-89.4091250351677,174.899139899188,-55.963463250108));
#19556=CARTESIAN_POINT('Ctrl Pts',(-89.5843332274473,174.841076361527,-55.7123912259186));
#19557=CARTESIAN_POINT('Ctrl Pts',(-89.7552435157444,174.784171529238,-55.4578272928341));
#19558=CARTESIAN_POINT('Ctrl Pts',(-89.9216547016079,174.728529608786,-55.1994155525535));
#19559=CARTESIAN_POINT('Ctrl Pts',(-90.0842201292001,174.674173571701,-54.9469757010161));
#19560=CARTESIAN_POINT('Ctrl Pts',(-90.2424920738752,174.621022683459,-54.6908638683083));
#19561=CARTESIAN_POINT('Ctrl Pts',(-90.3962399116234,174.569189839793,-54.4307284026853));
#19562=CARTESIAN_POINT('Ctrl Pts',(-90.4338181432748,174.556521130854,-54.3671474708747));
#19563=CARTESIAN_POINT('Ctrl Pts',(-90.4711259025328,174.543931237885,-54.3033260766955));
#19564=CARTESIAN_POINT('Ctrl Pts',(-90.5081594097971,174.531421964099,-54.2392588953588));
#19565=CARTESIAN_POINT('Ctrl Pts',(-90.6258211678479,174.491677871404,-54.0357065519191));
#19566=CARTESIAN_POINT('Ctrl Pts',(-90.7408707175398,174.452693862087,-53.829342570037));
#19567=CARTESIAN_POINT('Ctrl Pts',(-90.8528197264801,174.414652822771,-53.6206616697916));
#19568=CARTESIAN_POINT('Ctrl Pts',(-90.8770642398965,174.406414371204,-53.5754681755962));
#19569=CARTESIAN_POINT('Ctrl Pts',(-90.9011631887087,174.398220198498,-53.530166131445));
#19570=CARTESIAN_POINT('Ctrl Pts',(-90.9251113671707,174.390072250981,-53.484760763727));
#19571=CARTESIAN_POINT('Ctrl Pts',(-90.9870859608341,174.36898648292,-53.3672579140252));
#19572=CARTESIAN_POINT('Ctrl Pts',(-91.0479909645711,174.348231072408,-53.2491784445003));
#19573=CARTESIAN_POINT('Ctrl Pts',(-91.1077374489716,174.327839629328,-53.1306240306533));
#19574=CARTESIAN_POINT('Ctrl Pts',(-91.2675020972162,174.273312040576,-52.8136044701529));
#19575=CARTESIAN_POINT('Ctrl Pts',(-91.4188853491734,174.221422147604,-52.4935170045305));
#19576=CARTESIAN_POINT('Ctrl Pts',(-91.5616044369495,174.172333458547,-52.1701322125482));
#19577=CARTESIAN_POINT('Ctrl Pts',(-91.5858008658025,174.164011019055,-52.1153059294401));
#19578=CARTESIAN_POINT('Ctrl Pts',(-91.6097481465213,174.155769142893,-52.0603848529147));
#19579=CARTESIAN_POINT('Ctrl Pts',(-91.6334447650117,174.147608685332,-52.0053678440317));
#19580=CARTESIAN_POINT('Ctrl Pts',(-91.7693244902838,174.100815480134,-51.6898926189329));
#19581=CARTESIAN_POINT('Ctrl Pts',(-91.896975170158,174.056697446588,-51.3712649984069));
#19582=CARTESIAN_POINT('Ctrl Pts',(-92.0160413151778,174.015428122255,-51.0492598743207));
#19583=CARTESIAN_POINT('Ctrl Pts',(-92.0460469028125,174.005027933959,-50.9681120974444));
#19584=CARTESIAN_POINT('Ctrl Pts',(-92.0755070693359,173.99480875918,-50.8867497863239));
#19585=CARTESIAN_POINT('Ctrl Pts',(-92.1044156446447,173.984773576468,-50.8051692644594));
#19586=CARTESIAN_POINT('Ctrl Pts',(-92.2246834254259,173.943024401988,-50.4657714140016));
#19587=CARTESIAN_POINT('Ctrl Pts',(-92.3353783621527,173.904467096425,-50.1226731650209));
#19588=CARTESIAN_POINT('Ctrl Pts',(-92.4360240236092,173.86933179434,-49.7756598162833));
#19589=CARTESIAN_POINT('Ctrl Pts',(-92.441460980855,173.867433757878,-49.756913884134));
#19590=CARTESIAN_POINT('Ctrl Pts',(-92.4468686004058,173.865545712799,-49.7381565249075));
#19591=CARTESIAN_POINT('Ctrl Pts',(-92.4522468032086,173.863667697162,-49.7193877041164));
#19592=CARTESIAN_POINT('Ctrl Pts',(-92.5472941682945,173.830478090055,-49.3876919634805));
#19593=CARTESIAN_POINT('Ctrl Pts',(-92.6331595635202,173.800418977058,-49.0524173856645));
#19594=CARTESIAN_POINT('Ctrl Pts',(-92.7093120482644,173.773713629046,-48.7133594415447));
#19595=CARTESIAN_POINT('Ctrl Pts',(-92.7651362071759,173.7541370703,-48.4648104333761));
#19596=CARTESIAN_POINT('Ctrl Pts',(-92.8157399774473,173.736363111541,-48.2142281953996));
#19597=CARTESIAN_POINT('Ctrl Pts',(-92.8608978789791,173.720486412539,-47.9615295291183));
#19598=CARTESIAN_POINT('Ctrl Pts',(-92.8951771189541,173.7084344536,-47.7697066602743));
#19599=CARTESIAN_POINT('Ctrl Pts',(-92.9261641075478,173.697529207677,-47.5775127333407));
#19600=CARTESIAN_POINT('Ctrl Pts',(-92.9538384701856,173.687784900467,-47.3849592374246));
#19601=CARTESIAN_POINT('Ctrl Pts',(-93.011917690001,173.667334862727,-46.9808539302176));
#19602=CARTESIAN_POINT('Ctrl Pts',(-93.0554077638896,173.651998516184,-46.5751636385015));
#19603=CARTESIAN_POINT('Ctrl Pts',(-93.0840095834533,173.641905099212,-46.1679806000269));
#19604=CARTESIAN_POINT('Ctrl Pts',(-93.1112639346017,173.632287196064,-45.7799804769057));
#19605=CARTESIAN_POINT('Ctrl Pts',(-93.1249999999199,173.627429788604,-45.3906249750178));
#19606=CARTESIAN_POINT('Ctrl Pts',(-93.125,173.627429788614,-45.));
#19607=CARTESIAN_POINT('Origin',(-40.3363668356791,225.625863228014,34.2057557851749));
#19608=CARTESIAN_POINT('Origin',(-133.630782057879,206.966980183574,47.2669739162829));
#19609=CARTESIAN_POINT('Ctrl Pts',(-126.766717328043,172.646656534391,47.2669739162829));
#19610=CARTESIAN_POINT('Ctrl Pts',(-122.224200046663,173.555159990667,81.0113880065328));
#19611=CARTESIAN_POINT('Ctrl Pts',(-128.778107499175,206.966980183574,81.9289350498845));
#19612=CARTESIAN_POINT('Ctrl Pts',(-125.076099494732,172.984780101054,46.9474471457708));
#19613=CARTESIAN_POINT('Ctrl Pts',(-120.489909983146,173.820474755958,80.7685873976232));
#19614=CARTESIAN_POINT('Ctrl Pts',(-126.495773409643,207.423447001473,81.6094082773501));
#19615=CARTESIAN_POINT('Ctrl Pts',(-123.376736606944,173.279171828244,46.6262675599665));
#19616=CARTESIAN_POINT('Ctrl Pts',(-118.752370779924,174.039540392876,80.5253319092848));
#19617=CARTESIAN_POINT('Ctrl Pts',(-124.201633525813,207.820875830352,81.2882286936138));
#19618=CARTESIAN_POINT('Ctrl Pts',(-121.670898717897,173.529438457885,46.3038641989655));
#19619=CARTESIAN_POINT('Ctrl Pts',(-117.014194117273,174.212632196936,80.2819871764182));
#19620=CARTESIAN_POINT('Ctrl Pts',(-121.898752375479,208.15873578029,80.9658253325671));
#19621=CARTESIAN_POINT('Origin',(-126.751426934183,208.15873578029,46.3038641989655));
#19622=CARTESIAN_POINT('Ctrl Pts',(-108.033967922038,209.585728186396,80.0000000000001));
#19623=CARTESIAN_POINT('Ctrl Pts',(-107.806114264457,174.586469869815,80.0000000000001));
#19624=CARTESIAN_POINT('Ctrl Pts',(-107.806114264457,174.586469869815,45.));
#19625=CARTESIAN_POINT('Ctrl Pts',(-110.368245901848,209.565212620413,80.0000000000001));
#19626=CARTESIAN_POINT('Ctrl Pts',(-109.323233110512,174.576593058387,79.9946819507977));
#19627=CARTESIAN_POINT('Ctrl Pts',(-110.140392035487,174.571273155555,44.9999999999672));
#19628=CARTESIAN_POINT('Ctrl Pts',(-112.690630392194,209.434596373781,80.0816280345492));
#19629=CARTESIAN_POINT('Ctrl Pts',(-110.831769330981,174.542829711498,80.0133399191142));
#19630=CARTESIAN_POINT('Ctrl Pts',(-112.462776734607,174.474520378982,45.1101978466734));
#19631=CARTESIAN_POINT('Ctrl Pts',(-117.312108354281,208.957898622415,80.4044093761842));
#19632=CARTESIAN_POINT('Ctrl Pts',(-113.886869252213,174.421832152824,80.1038421117714));
#19633=CARTESIAN_POINT('Ctrl Pts',(-117.084254696706,174.121410933541,45.5459526578167));
#19634=CARTESIAN_POINT('Ctrl Pts',(-119.611215134957,208.611807682767,80.645570118894));
#19635=CARTESIAN_POINT('Ctrl Pts',(-115.428565673973,174.334921359983,80.1754126411297));
#19636=CARTESIAN_POINT('Ctrl Pts',(-119.383361285288,173.865047302731,45.8715196241861));
#19637=CARTESIAN_POINT('Ctrl Pts',(-121.898752375479,208.15873578029,80.965825332567));
#19638=CARTESIAN_POINT('Ctrl Pts',(-117.014194117272,174.212632196936,80.2819871764181));
#19639=CARTESIAN_POINT('Ctrl Pts',(-121.670898717897,173.529438457885,46.3038641989654));
#19640=CARTESIAN_POINT('Origin',(-108.033967922038,209.585728186396,45.));
#19641=CARTESIAN_POINT('Origin',(-107.155103814224,74.5885889652995,45.0000000000001));
#19642=CARTESIAN_POINT('Origin',(-93.0342906798268,208.848049102839,45.0000000000001));
#19643=CARTESIAN_POINT('Origin',(-115.,0.,45.0000000000001));
#19644=CARTESIAN_POINT('Ctrl Pts',(-93.125,173.627429788614,45.0000000000001));
#19645=CARTESIAN_POINT('Ctrl Pts',(-93.1249999998108,173.62742978859,45.5703854531217));
#19646=CARTESIAN_POINT('Ctrl Pts',(-93.0957247306423,173.637782029819,46.1351652243981));
#19647=CARTESIAN_POINT('Ctrl Pts',(-93.038653950843,173.657902731047,46.6946224880328));
#19648=CARTESIAN_POINT('Ctrl Pts',(-93.0151077973288,173.666204091596,46.9254422991599));
#19649=CARTESIAN_POINT('Ctrl Pts',(-92.986829698282,173.676168463279,47.155356013543));
#19650=CARTESIAN_POINT('Ctrl Pts',(-92.9539212025254,173.687755741858,47.384383122678));
#19651=CARTESIAN_POINT('Ctrl Pts',(-92.9273987437467,173.697094458545,47.5689665234563));
#19652=CARTESIAN_POINT('Ctrl Pts',(-92.8978677052669,173.707487484341,47.7529742044882));
#19653=CARTESIAN_POINT('Ctrl Pts',(-92.8653667429934,173.718915089093,47.9364143980648));
#19654=CARTESIAN_POINT('Ctrl Pts',(-92.8078734084644,173.739130216795,48.2609152028896));
#19655=CARTESIAN_POINT('Ctrl Pts',(-92.7410476493066,173.762598797023,48.5838620304402));
#19656=CARTESIAN_POINT('Ctrl Pts',(-92.6651291805777,173.789202135506,48.9050632039656));
#19657=CARTESIAN_POINT('Ctrl Pts',(-92.6008395531292,173.811730497162,49.177064261517));
#19658=CARTESIAN_POINT('Ctrl Pts',(-92.530030351504,173.836506504464,49.4478136279032));
#19659=CARTESIAN_POINT('Ctrl Pts',(-92.4528745253981,173.863448838665,49.7171990214557));
#19660=CARTESIAN_POINT('Ctrl Pts',(-92.3606101775622,173.895666974608,50.0393350014215));
#19661=CARTESIAN_POINT('Ctrl Pts',(-92.2592673536355,173.930983612063,50.3595200750698));
#19662=CARTESIAN_POINT('Ctrl Pts',(-92.1491224618084,173.969248257698,50.6775593968402));
#19663=CARTESIAN_POINT('Ctrl Pts',(-92.1374506250882,173.973303086648,50.7112613958408));
#19664=CARTESIAN_POINT('Ctrl Pts',(-92.1256799934841,173.977391005235,50.7449393065516));
#19665=CARTESIAN_POINT('Ctrl Pts',(-92.1138109280872,173.981511824407,50.7785929019537));
#19666=CARTESIAN_POINT('Ctrl Pts',(-92.0044728350165,174.019472901806,51.088610567473));
#19667=CARTESIAN_POINT('Ctrl Pts',(-91.8874014722842,174.060011293566,51.3948244481383));
#19668=CARTESIAN_POINT('Ctrl Pts',(-91.7630218111992,174.102936771868,51.697462505704));
#19669=CARTESIAN_POINT('Ctrl Pts',(-91.7213243161257,174.117327267101,51.7989200012811));
#19670=CARTESIAN_POINT('Ctrl Pts',(-91.6788050567026,174.131986213741,51.8999755541278));
#19671=CARTESIAN_POINT('Ctrl Pts',(-91.6354788602119,174.1469069512,52.0006375683561));
#19672=CARTESIAN_POINT('Ctrl Pts',(-91.5019434891281,174.192894053112,52.3108872674477));
#19673=CARTESIAN_POINT('Ctrl Pts',(-91.3607375382183,174.24136675191,52.6173978737244));
#19674=CARTESIAN_POINT('Ctrl Pts',(-91.2122219564331,174.292145465175,52.9204043353714));
#19675=CARTESIAN_POINT('Ctrl Pts',(-91.1788225996643,174.303564983183,52.9885468211238));
#19676=CARTESIAN_POINT('Ctrl Pts',(-91.145053372545,174.31510121109,53.05651205668));
#19677=CARTESIAN_POINT('Ctrl Pts',(-91.1109180542637,174.326752250885,53.1243026631603));
#19678=CARTESIAN_POINT('Ctrl Pts',(-91.0521049058449,174.346826308115,53.2411018963612));
#19679=CARTESIAN_POINT('Ctrl Pts',(-90.9921666735604,174.367253920307,53.3574364564119));
#19680=CARTESIAN_POINT('Ctrl Pts',(-90.9312096089697,174.387995830875,53.4731771255933));
#19681=CARTESIAN_POINT('Ctrl Pts',(-90.8246553600374,174.424253132909,53.6754942837171));
#19682=CARTESIAN_POINT('Ctrl Pts',(-90.7149851721648,174.461470136965,53.8759974934974));
#19683=CARTESIAN_POINT('Ctrl Pts',(-90.6027342996058,174.499449100598,54.074036380043));
#19684=CARTESIAN_POINT('Ctrl Pts',(-90.5725830611701,174.509650471527,54.1272307789074));
#19685=CARTESIAN_POINT('Ctrl Pts',(-90.5422454352643,174.519906887338,54.1802475882314));
#19686=CARTESIAN_POINT('Ctrl Pts',(-90.5117313782821,174.530214666933,54.233074650745));
#19687=CARTESIAN_POINT('Ctrl Pts',(-90.3527342599104,174.583924576873,54.5083363347816));
#19688=CARTESIAN_POINT('Ctrl Pts',(-90.1886986672789,174.63911456029,54.7790268575882));
#19689=CARTESIAN_POINT('Ctrl Pts',(-90.0199441738519,174.695636393522,55.0455065671526));
#19690=CARTESIAN_POINT('Ctrl Pts',(-89.8474021802967,174.753426794164,55.3179671067002));
#19691=CARTESIAN_POINT('Ctrl Pts',(-89.6699270040715,174.81260956482,55.5860256574295));
#19692=CARTESIAN_POINT('Ctrl Pts',(-89.4878140788683,174.87304413341,55.8500453507872));
#19693=CARTESIAN_POINT('Ctrl Pts',(-89.4637239539776,174.881038493522,55.8849702051295));
#19694=CARTESIAN_POINT('Ctrl Pts',(-89.4395526126323,174.889054782192,55.9198243558653));
#19695=CARTESIAN_POINT('Ctrl Pts',(-89.4153006812224,174.897092695787,55.9546086161183));
#19696=CARTESIAN_POINT('Ctrl Pts',(-89.319261936399,174.928923197019,56.0923558593315));
#19697=CARTESIAN_POINT('Ctrl Pts',(-89.2219626997243,174.961090994622,56.2290004746553));
#19698=CARTESIAN_POINT('Ctrl Pts',(-89.1234500151856,174.993574426559,56.3645787456421));
#19699=CARTESIAN_POINT('Ctrl Pts',(-88.899087950989,175.067555253247,56.6733574666893));
#19700=CARTESIAN_POINT('Ctrl Pts',(-88.6684301573737,175.143173436595,56.9766043214186));
#19701=CARTESIAN_POINT('Ctrl Pts',(-88.4319084098773,175.220215129991,57.2746888173799));
#19702=CARTESIAN_POINT('Ctrl Pts',(-88.190557746909,175.298829735092,57.578859116654));
#19703=CARTESIAN_POINT('Ctrl Pts',(-87.9431011781495,175.378926632654,57.8776540776403));
#19704=CARTESIAN_POINT('Ctrl Pts',(-87.6899520658236,175.460298134701,58.1714442031506));
#19705=CARTESIAN_POINT('Ctrl Pts',(-87.6281678364518,175.48015787468,58.2431473836789));
#19706=CARTESIAN_POINT('Ctrl Pts',(-87.5660443165453,175.50009362537,58.3145523435447));
#19707=CARTESIAN_POINT('Ctrl Pts',(-87.5035871237125,175.520102532267,58.3856642785872));
#19708=CARTESIAN_POINT('Ctrl Pts',(-87.2350633724273,175.606127319733,58.6913975767498));
#19709=CARTESIAN_POINT('Ctrl Pts',(-86.9603723263989,175.693503929557,58.9917147375286));
#19710=CARTESIAN_POINT('Ctrl Pts',(-86.6798569195729,175.782039633885,59.2869796049606));
#19711=CARTESIAN_POINT('Ctrl Pts',(-86.3937700864287,175.872333780499,59.5881088435223));
#19712=CARTESIAN_POINT('Ctrl Pts',(-86.1016251709388,175.96383360254,59.8839830696031));
#19713=CARTESIAN_POINT('Ctrl Pts',(-85.8037404597079,176.056353351122,60.1749661075604));
#19714=CARTESIAN_POINT('Ctrl Pts',(-85.7621131907888,176.0692823277,60.2156289167454));
#19715=CARTESIAN_POINT('Ctrl Pts',(-85.7203737644335,176.082231249576,60.2561961763065));
#19716=CARTESIAN_POINT('Ctrl Pts',(-85.6785229814522,176.095199636747,60.2966688461824));
#19717=CARTESIAN_POINT('Ctrl Pts',(-85.6755866033166,176.096109538207,60.2995085317138));
#19718=CARTESIAN_POINT('Ctrl Pts',(-85.6726496819324,176.097019533954,60.3023477467889));
#19719=CARTESIAN_POINT('Ctrl Pts',(-85.6697122175902,176.097929623816,60.3051864917303));
#19720=CARTESIAN_POINT('Ctrl Pts',(-85.4253294684895,176.173644674843,60.5413562667317));
#19721=CARTESIAN_POINT('Ctrl Pts',(-85.1768557609506,176.250107482301,60.7745219435438));
#19722=CARTESIAN_POINT('Ctrl Pts',(-84.9250673075622,176.327042272143,61.0043417974612));
#19723=CARTESIAN_POINT('Ctrl Pts',(-84.6640070957159,176.406810078268,61.2426244468155));
#19724=CARTESIAN_POINT('Ctrl Pts',(-84.3993834390816,176.48708530926,61.4773104469835));
#19725=CARTESIAN_POINT('Ctrl Pts',(-84.1320102189896,176.567577409112,61.7080365871725));
#19726=CARTESIAN_POINT('Ctrl Pts',(-83.9689546335988,176.616664922275,61.8487432212944));
#19727=CARTESIAN_POINT('Ctrl Pts',(-83.8048754731111,176.665833414535,61.9879774868914));
#19728=CARTESIAN_POINT('Ctrl Pts',(-83.6399487552332,176.71501976099,62.1256597309597));
#19729=CARTESIAN_POINT('Ctrl Pts',(-83.603725747223,176.72582260388,62.1558990099189));
#19730=CARTESIAN_POINT('Ctrl Pts',(-83.5674583869559,176.736627418291,62.1860681891631));
#19731=CARTESIAN_POINT('Ctrl Pts',(-83.5311469089632,176.747434063254,62.2161678518087));
#19732=CARTESIAN_POINT('Ctrl Pts',(-83.1608098696161,176.857649926731,62.5231512236161));
#19733=CARTESIAN_POINT('Ctrl Pts',(-82.7858618806584,176.968045925943,62.822898654204));
#19734=CARTESIAN_POINT('Ctrl Pts',(-82.4066290249949,177.078471627047,63.1159641240302));
#19735=CARTESIAN_POINT('Ctrl Pts',(-82.0307904452302,177.187908976824,63.4064065482892));
#19736=CARTESIAN_POINT('Ctrl Pts',(-81.6507431062853,177.29737565131,63.6902859085264));
#19737=CARTESIAN_POINT('Ctrl Pts',(-81.2667672330688,177.406739868464,63.9681105627763));
#19738=CARTESIAN_POINT('Ctrl Pts',(-80.8367583674063,177.529215227576,64.2792422581777));
#19739=CARTESIAN_POINT('Ctrl Pts',(-80.4017673145224,177.651546575252,64.5827722310067));
#19740=CARTESIAN_POINT('Ctrl Pts',(-79.9621900595459,177.773520712408,64.8792981054518));
#19741=CARTESIAN_POINT('Ctrl Pts',(-79.6949806088862,177.847666136939,65.0595497338513));
#19742=CARTESIAN_POINT('Ctrl Pts',(-79.4260757287456,177.921679850411,65.2372125436568));
#19743=CARTESIAN_POINT('Ctrl Pts',(-79.1555577084484,177.99551638268,65.4124146719346));
#19744=CARTESIAN_POINT('Ctrl Pts',(-78.6678978020531,178.128620700001,65.7282496517351));
#19745=CARTESIAN_POINT('Ctrl Pts',(-78.174974935409,178.261158296907,66.0360692211114));
#19746=CARTESIAN_POINT('Ctrl Pts',(-77.6770538946029,178.392947212377,66.3364299472173));
#19747=CARTESIAN_POINT('Ctrl Pts',(-77.2752739443468,178.499289663414,66.5787955186708));
#19748=CARTESIAN_POINT('Ctrl Pts',(-76.8702388268825,178.605144922234,66.8163038125245));
#19749=CARTESIAN_POINT('Ctrl Pts',(-76.4620699385986,178.710422801494,67.0492309684832));
#19750=CARTESIAN_POINT('Ctrl Pts',(-75.7676341385142,178.88953671834,67.4455202510635));
#19751=CARTESIAN_POINT('Ctrl Pts',(-75.0640159311286,179.067016755113,67.8286240092616));
#19752=CARTESIAN_POINT('Ctrl Pts',(-74.3523513864555,179.242262974854,68.1994629803233));
#19753=CARTESIAN_POINT('Ctrl Pts',(-74.3001475880404,179.255118074067,68.2266656884457));
#19754=CARTESIAN_POINT('Ctrl Pts',(-74.2479004819618,179.267961168359,68.2538023873426));
#19755=CARTESIAN_POINT('Ctrl Pts',(-74.1956105112451,179.280792028091,68.2808734338598));
#19756=CARTESIAN_POINT('Ctrl Pts',(-74.1106840385824,179.301631199414,68.3248407274056));
#19757=CARTESIAN_POINT('Ctrl Pts',(-74.0256241492911,179.32244285591,68.3686431530313));
#19758=CARTESIAN_POINT('Ctrl Pts',(-73.9404393252445,179.343224564154,68.4122787524547));
#19759=CARTESIAN_POINT('Ctrl Pts',(-73.4939121922517,179.452159420861,68.6410105638429));
#19760=CARTESIAN_POINT('Ctrl Pts',(-73.0437861609672,179.560317898584,68.865252552359));
#19761=CARTESIAN_POINT('Ctrl Pts',(-72.5909626258734,179.6674285339,69.0848598562164));
#19762=CARTESIAN_POINT('Ctrl Pts',(-72.2477173132217,179.748619595445,69.2513246528342));
#19763=CARTESIAN_POINT('Ctrl Pts',(-71.9029207067315,179.829208827108,69.4151263648389));
#19764=CARTESIAN_POINT('Ctrl Pts',(-71.5569461393784,179.909080577907,69.5761985292671));
#19765=CARTESIAN_POINT('Ctrl Pts',(-71.4878049613763,179.925042522687,69.6083879450301));
#19766=CARTESIAN_POINT('Ctrl Pts',(-71.418625045659,179.94097409477,69.6404652116115));
#19767=CARTESIAN_POINT('Ctrl Pts',(-71.3494059445144,179.956875294743,69.6724315951806));
#19768=CARTESIAN_POINT('Ctrl Pts',(-70.620066360206,180.12442116556,70.0092511799283));
#19769=CARTESIAN_POINT('Ctrl Pts',(-69.8860898581444,180.288658175961,70.3338945491597));
#19770=CARTESIAN_POINT('Ctrl Pts',(-69.1478094783436,180.449378512452,70.6473765849958));
#19771=CARTESIAN_POINT('Ctrl Pts',(-69.047516772658,180.471211785889,70.6899619799461));
#19772=CARTESIAN_POINT('Ctrl Pts',(-68.9471446035588,180.492980167431,70.7323413329162));
#19773=CARTESIAN_POINT('Ctrl Pts',(-68.8466937699905,180.514683141084,70.7745171247771));
#19774=CARTESIAN_POINT('Ctrl Pts',(-68.0582330320637,180.685034565894,71.1055642131092));
#19775=CARTESIAN_POINT('Ctrl Pts',(-67.2649492078607,180.851347580507,71.4241092502634));
#19776=CARTESIAN_POINT('Ctrl Pts',(-66.4670699960451,181.013433614092,71.7310838367989));
#19777=CARTESIAN_POINT('Ctrl Pts',(-66.3245219996644,181.04239168066,71.7859274918314));
#19778=CARTESIAN_POINT('Ctrl Pts',(-66.1818272575054,181.071214828723,71.8404017138963));
#19779=CARTESIAN_POINT('Ctrl Pts',(-66.0389869830734,181.099901984681,71.8945116652855));
#19780=CARTESIAN_POINT('Ctrl Pts',(-65.1193399688903,181.284598194672,72.2428871877396));
#19781=CARTESIAN_POINT('Ctrl Pts',(-64.1936684744158,181.463650393234,72.5761611402097));
#19782=CARTESIAN_POINT('Ctrl Pts',(-63.2624005133239,181.63674053216,72.8956249559814));
#19783=CARTESIAN_POINT('Ctrl Pts',(-62.376972362934,181.801310653719,73.1993638016555));
#19784=CARTESIAN_POINT('Ctrl Pts',(-61.486474404333,181.960496756059,73.4906000796016));
#19785=CARTESIAN_POINT('Ctrl Pts',(-60.5910895271308,182.114088224847,73.7701318404769));
#19786=CARTESIAN_POINT('Ctrl Pts',(-59.5604150468438,182.290886841063,74.0918998976549));
#19787=CARTESIAN_POINT('Ctrl Pts',(-58.5232783791325,182.460276659765,74.3981595579253));
#19788=CARTESIAN_POINT('Ctrl Pts',(-57.4800356321375,182.621919491696,74.6900461765216));
#19789=CARTESIAN_POINT('Ctrl Pts',(-56.6637510422464,182.748396817469,74.9184326660917));
#19790=CARTESIAN_POINT('Ctrl Pts',(-55.8437232434193,182.870134019457,75.1380109600897));
#19791=CARTESIAN_POINT('Ctrl Pts',(-55.0200356674394,182.986992560819,75.3491798901418));
#19792=CARTESIAN_POINT('Ctrl Pts',(-54.0818398570834,183.120096661338,75.5897053165653));
#19793=CARTESIAN_POINT('Ctrl Pts',(-53.138916039872,183.246879328694,75.8193215249152));
#19794=CARTESIAN_POINT('Ctrl Pts',(-52.1914100346049,183.367125045976,76.0385873974286));
#19795=CARTESIAN_POINT('Ctrl Pts',(-51.9664874968378,183.39566942642,76.0906375545963));
#19796=CARTESIAN_POINT('Ctrl Pts',(-51.7412873445566,183.423847988172,76.1421089209594));
#19797=CARTESIAN_POINT('Ctrl Pts',(-51.5158017905921,183.451658932195,76.1930106956108));
#19798=CARTESIAN_POINT('Ctrl Pts',(-50.7914095839582,183.54100403992,76.3565371309545));
#19799=CARTESIAN_POINT('Ctrl Pts',(-50.0648491243609,183.626445028928,76.5139745559305));
#19800=CARTESIAN_POINT('Ctrl Pts',(-49.3379841963483,183.707748524837,76.6652222472324));
#19801=CARTESIAN_POINT('Ctrl Pts',(-49.0517710051111,183.739762908977,76.7247781326885));
#19802=CARTESIAN_POINT('Ctrl Pts',(-48.765428864529,183.771145312749,76.7833912188635));
#19803=CARTESIAN_POINT('Ctrl Pts',(-48.4790950286481,183.801877303775,76.8410480177466));
#19804=CARTESIAN_POINT('Ctrl Pts',(-47.465412426358,183.910675080124,77.0451653332976));
#19805=CARTESIAN_POINT('Ctrl Pts',(-46.4501431481726,184.011533733904,77.2376834765327));
#19806=CARTESIAN_POINT('Ctrl Pts',(-45.4334520952105,184.104382640783,77.4192426182608));
#19807=CARTESIAN_POINT('Ctrl Pts',(-43.9614743671191,184.23881042256,77.6821061618874));
#19808=CARTESIAN_POINT('Ctrl Pts',(-42.4865233282392,184.35644859137,77.9220388612771));
#19809=CARTESIAN_POINT('Ctrl Pts',(-41.0090296046946,184.457102613407,78.1405824168399));
#19810=CARTESIAN_POINT('Ctrl Pts',(-40.4460861266667,184.495453047212,78.2238502286137));
#19811=CARTESIAN_POINT('Ctrl Pts',(-39.882773587587,184.531338201069,78.3040134129349));
#19812=CARTESIAN_POINT('Ctrl Pts',(-39.3191160265197,184.564748496546,78.3811587995839));
#19813=CARTESIAN_POINT('Ctrl Pts',(-38.8279492645467,184.593861965041,78.4483826822721));
#19814=CARTESIAN_POINT('Ctrl Pts',(-38.3365224616305,184.621097710092,78.5133267944161));
#19815=CARTESIAN_POINT('Ctrl Pts',(-37.8448477983021,184.646448347107,78.5760264393378));
#19816=CARTESIAN_POINT('Ctrl Pts',(-35.8495579567748,184.749325050514,78.8304710424678));
#19817=CARTESIAN_POINT('Ctrl Pts',(-33.8497806197686,184.821222887997,79.0480140922849));
#19818=CARTESIAN_POINT('Ctrl Pts',(-31.8457500386124,184.861652872759,79.2310642129745));
#19819=CARTESIAN_POINT('Ctrl Pts',(-30.2338968514672,184.894170939303,79.3782924654847));
#19820=CARTESIAN_POINT('Ctrl Pts',(-28.6192924766604,184.906332737617,79.5032079101486));
#19821=CARTESIAN_POINT('Ctrl Pts',(-27.0020640562796,184.897899772955,79.6070815377235));
#19822=CARTESIAN_POINT('Ctrl Pts',(-26.7516674121844,184.896594090947,79.623164366486));
#19823=CARTESIAN_POINT('Ctrl Pts',(-26.5012074979132,184.89479493717,79.6387417725125));
#19824=CARTESIAN_POINT('Ctrl Pts',(-26.2506843886171,184.892501020704,79.6538158669559));
#19825=CARTESIAN_POINT('Ctrl Pts',(-24.2925620301514,184.874571460701,79.7716370190483));
#19826=CARTESIAN_POINT('Ctrl Pts',(-22.3305986235038,184.826447634977,79.8587103330367));
#19827=CARTESIAN_POINT('Ctrl Pts',(-20.364880005263,184.747551715547,79.9160570352638));
#19828=CARTESIAN_POINT('Ctrl Pts',(-18.4352480461297,184.670104167273,79.9723509668274));
#19829=CARTESIAN_POINT('Ctrl Pts',(-16.5019975076899,184.563003946033,80.));
#19830=CARTESIAN_POINT('Ctrl Pts',(-14.5652173913043,184.425742352699,80.));
#19831=CARTESIAN_POINT('Origin',(3.92135447228743,250.,-28.0096748020595));
#19832=CARTESIAN_POINT('Origin',(-126.751426934183,250.,-46.3038641989653));
#19833=CARTESIAN_POINT('Origin',(-108.033967922038,250.,-180.));
#19834=CARTESIAN_POINT('Origin',(-115.000000000001,250.,-45.1798442476466));
#19835=CARTESIAN_POINT('Ctrl Pts',(-108.033967922038,249.902929948988,-79.9999999999999));
#19836=CARTESIAN_POINT('Ctrl Pts',(-107.058723431124,284.889340141846,-79.9999999999999));
#19837=CARTESIAN_POINT('Ctrl Pts',(-107.058723431124,284.889340141846,-44.9999999999999));
#19838=CARTESIAN_POINT('Ctrl Pts',(-109.754786521379,249.96768639131,-79.9999999999999));
#19839=CARTESIAN_POINT('Ctrl Pts',(-109.104754181425,284.946373149815,-79.9832218312162));
#19840=CARTESIAN_POINT('Ctrl Pts',(-109.707063739997,284.963162499786,-44.9999999999515));
#19841=CARTESIAN_POINT('Ctrl Pts',(-111.474797972355,250.000000000097,-80.0443888208499));
#19842=CARTESIAN_POINT('Ctrl Pts',(-111.151224324472,284.983237668963,-80.027670071346));
#19843=CARTESIAN_POINT('Ctrl Pts',(-112.354160313521,285.,-45.0599248824912));
#19844=CARTESIAN_POINT('Ctrl Pts',(-113.193991683492,250.,-80.1332179612197));
#19845=CARTESIAN_POINT('Ctrl Pts',(-113.193991683492,285.,-80.1332179612197));
#19846=CARTESIAN_POINT('Ctrl Pts',(-115.000000000001,285.,-45.1798442476466));
#19847=CARTESIAN_POINT('Origin',(-108.033967922038,249.902929948988,-44.9999999999999));
#19848=CARTESIAN_POINT('Origin',(-115.,0.,-44.9999999999999));
#19849=CARTESIAN_POINT('Ctrl Pts',(170.,0.,-45.));
#19850=CARTESIAN_POINT('Ctrl Pts',(170.,1.10014726515156,-45.2609231886251));
#19851=CARTESIAN_POINT('Ctrl Pts',(169.99070766613,2.20035818324513,-45.521861500102));
#19852=CARTESIAN_POINT('Ctrl Pts',(169.972146497345,3.29972358349869,-45.7825844101657));
#19853=CARTESIAN_POINT('Ctrl Pts',(169.953585328561,4.39908898375224,-46.0433073202294));
#19854=CARTESIAN_POINT('Ctrl Pts',(169.925755342586,5.4976087048996,-46.303814771838));
#19855=CARTESIAN_POINT('Ctrl Pts',(169.888733367566,6.59437588114246,-46.5638770533837));
#19856=CARTESIAN_POINT('Ctrl Pts',(169.830507889234,8.31929178364157,-46.9728841560716));
#19857=CARTESIAN_POINT('Ctrl Pts',(169.749525512653,10.040940545513,-47.3810433083307));
#19858=CARTESIAN_POINT('Ctrl Pts',(169.645957717126,11.7593577335116,-47.7883060136141));
#19859=CARTESIAN_POINT('Ctrl Pts',(169.617820820864,12.2262106379944,-47.8989495629087));
#19860=CARTESIAN_POINT('Ctrl Pts',(169.588016647507,12.6928250667316,-48.0095269576643));
#19861=CARTESIAN_POINT('Ctrl Pts',(169.556547977067,13.1592018092437,-48.1200372424757));
#19862=CARTESIAN_POINT('Ctrl Pts',(169.439189829893,14.8984907471084,-48.5321703922921));
#19863=CARTESIAN_POINT('Ctrl Pts',(169.298685536974,16.6344752969574,-48.9433703105389));
#19864=CARTESIAN_POINT('Ctrl Pts',(169.13514695613,18.3671801914865,-49.353583556718));
#19865=CARTESIAN_POINT('Ctrl Pts',(168.971189618771,20.1043218461985,-49.7648471939953));
#19866=CARTESIAN_POINT('Ctrl Pts',(168.784079857552,21.8381673450186,-50.1751192500177));
#19867=CARTESIAN_POINT('Ctrl Pts',(168.573878051586,23.5687409239769,-50.5843439701539));
#19868=CARTESIAN_POINT('Ctrl Pts',(168.467429473832,24.44512300515,-50.7915800081133));
#19869=CARTESIAN_POINT('Ctrl Pts',(168.355058055932,25.3206659538579,-50.9985474099555));
#19870=CARTESIAN_POINT('Ctrl Pts',(168.236766577472,26.1953724560961,-51.205238561613));
#19871=CARTESIAN_POINT('Ctrl Pts',(168.005816599942,27.9031323866398,-51.6087783385501));
#19872=CARTESIAN_POINT('Ctrl Pts',(167.752307699827,29.6076802919403,-52.0112562037791));
#19873=CARTESIAN_POINT('Ctrl Pts',(167.476221608132,31.3090471360765,-52.41262057382));
#19874=CARTESIAN_POINT('Ctrl Pts',(167.195655370704,33.0380226560489,-52.8204980241076));
#19875=CARTESIAN_POINT('Ctrl Pts',(166.891773307017,34.7637133896723,-53.2272257253356));
#19876=CARTESIAN_POINT('Ctrl Pts',(166.564503212267,36.4861388550054,-53.6327416763463));
#19877=CARTESIAN_POINT('Ctrl Pts',(166.243285658137,38.1767097443699,-54.0307580060799));
#19878=CARTESIAN_POINT('Ctrl Pts',(165.899536888957,39.8641352719207,-54.4276071116183));
#19879=CARTESIAN_POINT('Ctrl Pts',(165.533140039383,41.5484171429918,-54.8232207088668));
#19880=CARTESIAN_POINT('Ctrl Pts',(165.156387442808,43.2803031268083,-55.2300158278135));
#19881=CARTESIAN_POINT('Ctrl Pts',(164.755688530513,45.0088656611518,-55.6355048330746));
#19882=CARTESIAN_POINT('Ctrl Pts',(164.330865112352,46.7340834604885,-56.0396004742571));
#19883=CARTESIAN_POINT('Ctrl Pts',(163.90604169419,48.4593012598251,-56.4436961154396));
#19884=CARTESIAN_POINT('Ctrl Pts',(163.45709360351,50.1811746454788,-56.8463985627328));
#19885=CARTESIAN_POINT('Ctrl Pts',(162.983793115997,51.8996540346802,-57.247604850381));
#19886=CARTESIAN_POINT('Ctrl Pts',(162.743229120032,52.7731039460092,-57.4515255948328));
#19887=CARTESIAN_POINT('Ctrl Pts',(162.496214958299,53.6462315733819,-57.6551905253493));
#19888=CARTESIAN_POINT('Ctrl Pts',(162.24298557228,54.5180618389271,-57.8583595275675));
#19889=CARTESIAN_POINT('Ctrl Pts',(161.989773057244,55.389834020243,-58.0615149939917));
#19890=CARTESIAN_POINT('Ctrl Pts',(161.730346187712,56.2603088858134,-58.2641745489658));
#19891=CARTESIAN_POINT('Ctrl Pts',(161.464989360853,57.1285269958721,-58.4661036377234));
#19892=CARTESIAN_POINT('Ctrl Pts',(161.351122831121,57.501085653638,-58.5527528672197));
#19893=CARTESIAN_POINT('Ctrl Pts',(161.236165016502,57.8732289727676,-58.6392676671293));
#19894=CARTESIAN_POINT('Ctrl Pts',(161.120141148337,58.2448821043678,-58.7256298498529));
#19895=CARTESIAN_POINT('Ctrl Pts',(160.604746227511,59.8958194448209,-59.109263243839));
#19896=CARTESIAN_POINT('Ctrl Pts',(160.068164227368,61.5375939752252,-59.4900027127986));
#19897=CARTESIAN_POINT('Ctrl Pts',(159.510544723069,63.1702864707303,-59.8677910350757));
#19898=CARTESIAN_POINT('Ctrl Pts',(159.357543388526,63.6182696004155,-59.9714497432759));
#19899=CARTESIAN_POINT('Ctrl Pts',(159.202957931221,64.065568921102,-60.0748862162546));
#19900=CARTESIAN_POINT('Ctrl Pts',(159.046790785211,64.512185956635,-60.1780991408196));
#19901=CARTESIAN_POINT('Ctrl Pts',(158.473786608197,66.1509008427348,-60.5568051517102));
#19902=CARTESIAN_POINT('Ctrl Pts',(157.879492825345,67.7804313129569,-60.9325012513163));
#19903=CARTESIAN_POINT('Ctrl Pts',(157.263999454076,69.400834013756,-61.3051178093134));
#19904=CARTESIAN_POINT('Ctrl Pts',(156.646365385725,71.0268725044679,-61.6790303344413));
#19905=CARTESIAN_POINT('Ctrl Pts',(156.007383843491,72.6437198968175,-62.0498420154008));
#19906=CARTESIAN_POINT('Ctrl Pts',(155.347098296672,74.2514158971068,-62.417468623946));
#19907=CARTESIAN_POINT('Ctrl Pts',(154.999559111842,75.0976215426612,-62.6109677130468));
#19908=CARTESIAN_POINT('Ctrl Pts',(154.646117068505,75.9412915600981,-62.8035841611313));
#19909=CARTESIAN_POINT('Ctrl Pts',(154.286773495438,76.782429413302,-62.9953039280719));
#19910=CARTESIAN_POINT('Ctrl Pts',(153.622311759971,78.3377763280565,-63.3498127007693));
#19911=CARTESIAN_POINT('Ctrl Pts',(152.937691679161,79.8844384046647,-63.7012418382629));
#19912=CARTESIAN_POINT('Ctrl Pts',(152.232871611383,81.4224500704914,-64.0495114541217));
#19913=CARTESIAN_POINT('Ctrl Pts',(151.495567436294,83.0313464035976,-64.4138322979342));
#19914=CARTESIAN_POINT('Ctrl Pts',(150.736158474361,84.6307770714895,-64.7746960106424));
#19915=CARTESIAN_POINT('Ctrl Pts',(149.954550021439,86.2207499804614,-65.1319884530789));
#19916=CARTESIAN_POINT('Ctrl Pts',(149.207970829692,87.7394652461946,-65.4732681589137));
#19917=CARTESIAN_POINT('Ctrl Pts',(148.441136834072,89.249551468873,-65.8112895102483));
#19918=CARTESIAN_POINT('Ctrl Pts',(147.653928142943,90.7509847859831,-66.1459310078955));
#19919=CARTESIAN_POINT('Ctrl Pts',(146.867822914329,92.2503134828016,-66.4801034249128));
#19920=CARTESIAN_POINT('Ctrl Pts',(146.061399808802,93.741013693034,-66.8109055943775));
#19921=CARTESIAN_POINT('Ctrl Pts',(145.234506851664,95.223028803549,-67.1381929309409));
#19922=CARTESIAN_POINT('Ctrl Pts',(144.40981406396,96.7011006172698,-67.4646094321829));
#19923=CARTESIAN_POINT('Ctrl Pts',(143.564759931134,98.1705336376485,-67.787529909235));
#19924=CARTESIAN_POINT('Ctrl Pts',(142.699165309371,99.6312365631214,-68.1067854529431));
#19925=CARTESIAN_POINT('Ctrl Pts',(142.57208263001,99.8456903465111,-68.1536571049555));
#19926=CARTESIAN_POINT('Ctrl Pts',(142.444557159281,100.059955890433,-68.2004497132391));
#19927=CARTESIAN_POINT('Ctrl Pts',(142.316588284338,100.274032839058,-68.247162694269));
#19928=CARTESIAN_POINT('Ctrl Pts',(141.487458133348,101.661070529399,-68.5498233297682));
#19929=CARTESIAN_POINT('Ctrl Pts',(140.639691681384,103.040221704901,-68.8491578079982));
#19930=CARTESIAN_POINT('Ctrl Pts',(139.77305998302,104.411420051739,-69.1450170053095));
#19931=CARTESIAN_POINT('Ctrl Pts',(139.453130089157,104.917618177652,-69.2542377986095));
#19932=CARTESIAN_POINT('Ctrl Pts',(139.130628954756,105.422732104968,-69.362984704975));
#19933=CARTESIAN_POINT('Ctrl Pts',(138.805544276616,105.926757191782,-69.4712492655195));
#19934=CARTESIAN_POINT('Ctrl Pts',(138.20270440341,106.861425725427,-69.6720160144317));
#19935=CARTESIAN_POINT('Ctrl Pts',(137.591646601873,107.79130568966,-69.8709000606912));
#19936=CARTESIAN_POINT('Ctrl Pts',(136.972927262067,108.715551339406,-70.0676789932748));
#19937=CARTESIAN_POINT('Ctrl Pts',(136.354207922262,109.639796989153,-70.2644579258585));
#19938=CARTESIAN_POINT('Ctrl Pts',(135.727827192656,110.558408197228,-70.4591316805119));
#19939=CARTESIAN_POINT('Ctrl Pts',(135.094388092976,111.470576450946,-70.6514912337012));
#19940=CARTESIAN_POINT('Ctrl Pts',(134.118891433214,112.875316204291,-70.9477250811292));
#19941=CARTESIAN_POINT('Ctrl Pts',(133.125836160857,114.265989764737,-71.2387250091251));
#19942=CARTESIAN_POINT('Ctrl Pts',(132.115279202864,115.642677372998,-71.5243588974733));
#19943=CARTESIAN_POINT('Ctrl Pts',(131.100057726306,117.025719481967,-71.8113112118284));
#19944=CARTESIAN_POINT('Ctrl Pts',(130.067172320333,118.394646372545,-72.0928479988192));
#19945=CARTESIAN_POINT('Ctrl Pts',(129.01664787406,119.74950996065,-72.3688065526259));
#19946=CARTESIAN_POINT('Ctrl Pts',(128.396773300342,120.54896350226,-72.5316392135045));
#19947=CARTESIAN_POINT('Ctrl Pts',(127.770756687264,121.34352001057,-72.6925291275462));
#19948=CARTESIAN_POINT('Ctrl Pts',(127.138598490159,122.133185094108,-72.851437859478));
#19949=CARTESIAN_POINT('Ctrl Pts',(126.121677576623,123.403479368257,-73.107066298032));
#19950=CARTESIAN_POINT('Ctrl Pts',(125.08890734821,124.66109427067,-73.3575491477337));
#19951=CARTESIAN_POINT('Ctrl Pts',(124.040215967679,125.906056570587,-73.6027362667229));
#19952=CARTESIAN_POINT('Ctrl Pts',(122.990840610091,127.151830859297,-73.848083301553));
#19953=CARTESIAN_POINT('Ctrl Pts',(121.92552299743,128.384936090349,-74.0881278349307));
#19954=CARTESIAN_POINT('Ctrl Pts',(120.844170049389,129.605365540767,-74.3226855021703));
#19955=CARTESIAN_POINT('Ctrl Pts',(119.763137083678,130.825433854834,-74.5571737616287));
#19956=CARTESIAN_POINT('Ctrl Pts',(118.66607793164,132.03283390954,-74.7861785321864));
#19957=CARTESIAN_POINT('Ctrl Pts',(117.552883524561,133.22752491456,-75.009479697586));
#19958=CARTESIAN_POINT('Ctrl Pts',(116.440807254544,134.42101592407,-75.2325565703488));
#19959=CARTESIAN_POINT('Ctrl Pts',(115.312627779448,135.601823387615,-75.4499414111029));
#19960=CARTESIAN_POINT('Ctrl Pts',(114.16822546943,136.769872585367,-75.6613770385435));
#19961=CARTESIAN_POINT('Ctrl Pts',(113.026415571553,137.935275803733,-75.8723337013029));
#19962=CARTESIAN_POINT('Ctrl Pts',(111.868455902192,139.087978438965,-76.0773681795067));
#19963=CARTESIAN_POINT('Ctrl Pts',(110.694222039097,140.227872886939,-76.2761857732088));
#19964=CARTESIAN_POINT('Ctrl Pts',(110.16402252702,140.742567190288,-76.3659574911657));
#19965=CARTESIAN_POINT('Ctrl Pts',(109.63050502821,141.25464974426,-76.4544611843318));
#19966=CARTESIAN_POINT('Ctrl Pts',(109.093658009703,141.764108460991,-76.5416670048306));
#19967=CARTESIAN_POINT('Ctrl Pts',(108.281664476563,142.534676554184,-76.6735678254667));
#19968=CARTESIAN_POINT('Ctrl Pts',(107.461568433179,143.299677084708,-76.80258103617));
#19969=CARTESIAN_POINT('Ctrl Pts',(106.634043305536,144.058369920031,-76.9284826090685));
#19970=CARTESIAN_POINT('Ctrl Pts',(105.806518177894,144.817062755354,-77.054384181967));
#19971=CARTESIAN_POINT('Ctrl Pts',(104.971564130646,145.569447788168,-77.1771740451513));
#19972=CARTESIAN_POINT('Ctrl Pts',(104.129891430385,146.314830427712,-77.2966438182492));
#19973=CARTESIAN_POINT('Ctrl Pts',(102.881043322562,147.420806300174,-77.473909399073));
#19974=CARTESIAN_POINT('Ctrl Pts',(101.619608187914,148.509435764892,-77.643559231171));
#19975=CARTESIAN_POINT('Ctrl Pts',(100.345654535066,149.580844722008,-77.8053456962242));
#19976=CARTESIAN_POINT('Ctrl Pts',(99.9024225601615,149.953607661172,-77.8616341916949));
#19977=CARTESIAN_POINT('Ctrl Pts',(99.4576751258032,150.324285878761,-77.9169704642455));
#19978=CARTESIAN_POINT('Ctrl Pts',(99.011414756953,150.692883965256,-77.971342843451));
#19979=CARTESIAN_POINT('Ctrl Pts',(97.7693082210675,151.718827840867,-78.1226811479409));
#19980=CARTESIAN_POINT('Ctrl Pts',(96.5154925721465,152.728661615878,-78.2665514875638));
#19981=CARTESIAN_POINT('Ctrl Pts',(95.2499812988189,153.722453132978,-78.4026874034882));
#19982=CARTESIAN_POINT('Ctrl Pts',(93.9839970223882,154.716616094001,-78.538874202176));
#19983=CARTESIAN_POINT('Ctrl Pts',(92.7063079976469,155.694724630978,-78.6673208962488));
#19984=CARTESIAN_POINT('Ctrl Pts',(91.416924495997,156.656823856401,-78.7877139697859));
#19985=CARTESIAN_POINT('Ctrl Pts',(90.4071022541114,157.410322870069,-78.8820036851973));
#19986=CARTESIAN_POINT('Ctrl Pts',(89.3901067970427,158.154001691191,-78.9713526037555));
#19987=CARTESIAN_POINT('Ctrl Pts',(88.3659439434344,158.887873384098,-79.0555895260508));
#19988=CARTESIAN_POINT('Ctrl Pts',(87.1437413180917,159.763651983738,-79.1561151282217));
#19989=CARTESIAN_POINT('Ctrl Pts',(85.9113392665142,160.62546502764,-79.2493608525903));
#19990=CARTESIAN_POINT('Ctrl Pts',(84.6686824263498,161.473300644551,-79.3350129070214));
#19991=CARTESIAN_POINT('Ctrl Pts',(83.4331570535623,162.316270628531,-79.4201734139776));
#19992=CARTESIAN_POINT('Ctrl Pts',(82.1874939418069,163.145422894328,-79.497827189361));
#19993=CARTESIAN_POINT('Ctrl Pts',(80.9316483599466,163.960729856028,-79.5676180305605));
#19994=CARTESIAN_POINT('Ctrl Pts',(79.689772071307,164.766967818978,-79.6366325591792));
#19995=CARTESIAN_POINT('Ctrl Pts',(78.4379383029592,165.55966648192,-79.6979580775793));
#19996=CARTESIAN_POINT('Ctrl Pts',(77.1761176725809,166.338787716879,-79.751203332978));
#19997=CARTESIAN_POINT('Ctrl Pts',(76.0053484983634,167.061688502386,-79.8006064749092));
#19998=CARTESIAN_POINT('Ctrl Pts',(74.8259920696566,167.772903562918,-79.8430528496191));
#19999=CARTESIAN_POINT('Ctrl Pts',(73.6379472668019,168.472368248304,-79.8781987072658));
#20000=CARTESIAN_POINT('Ctrl Pts',(72.4567121022887,169.167823740157,-79.9131431157927));
#20001=CARTESIAN_POINT('Ctrl Pts',(71.2668876275958,169.851662875256,-79.9408704679589));
#20002=CARTESIAN_POINT('Ctrl Pts',(70.0683926518377,170.523813905937,-79.9609955712169));
#20003=CARTESIAN_POINT('Ctrl Pts',(68.8812223363898,171.189613735943,-79.9809305110094));
#20004=CARTESIAN_POINT('Ctrl Pts',(67.6855443847963,171.843944978397,-79.9934061572428));
#20005=CARTESIAN_POINT('Ctrl Pts',(66.481301251357,172.486734441791,-79.9980017915023));
#20006=CARTESIAN_POINT('Ctrl Pts',(66.1331776656422,172.672552543338,-79.9993303011966));
#20007=CARTESIAN_POINT('Ctrl Pts',(65.7843384560529,172.857406119814,-80.));
#20008=CARTESIAN_POINT('Ctrl Pts',(65.4347826086956,173.041293409847,-80.));
#20009=CARTESIAN_POINT('Origin',(3.92135447228745,250.,28.0096748020596));
#20010=CARTESIAN_POINT('Origin',(-126.751426934183,250.,46.3038641989655));
#20011=CARTESIAN_POINT('Origin',(-108.033967922038,250.,180.));
#20012=CARTESIAN_POINT('Origin',(-115.000000000001,250.,45.1798442476468));
#20013=CARTESIAN_POINT('Ctrl Pts',(-113.193991683492,250.,80.1332179612198));
#20014=CARTESIAN_POINT('Ctrl Pts',(-113.193991683492,285.,80.1332179612198));
#20015=CARTESIAN_POINT('Ctrl Pts',(-115.000000000001,285.,45.1798442476468));
#20016=CARTESIAN_POINT('Ctrl Pts',(-111.474797972362,250.000000000097,80.0443888208503));
#20017=CARTESIAN_POINT('Ctrl Pts',(-111.151224324474,284.983237668963,80.0276700713582));
#20018=CARTESIAN_POINT('Ctrl Pts',(-112.354160313515,285.,45.0599248825255));
#20019=CARTESIAN_POINT('Ctrl Pts',(-109.754786521371,249.967686391406,80.0000000000001));
#20020=CARTESIAN_POINT('Ctrl Pts',(-109.104754181423,284.946373149817,79.9832218311837));
#20021=CARTESIAN_POINT('Ctrl Pts',(-109.707063740001,284.963162499787,44.9999999999839));
#20022=CARTESIAN_POINT('Ctrl Pts',(-108.033967922038,249.902929948988,80.0000000000001));
#20023=CARTESIAN_POINT('Ctrl Pts',(-107.058723431124,284.889340141846,80.0000000000001));
#20024=CARTESIAN_POINT('Ctrl Pts',(-107.058723431124,284.889340141846,45.0000000000001));
#20025=CARTESIAN_POINT('Origin',(-108.033967922038,249.902929948988,45.0000000000001));
#20026=CARTESIAN_POINT('Origin',(-115.,0.,45.0000000000001));
#20027=CARTESIAN_POINT('Ctrl Pts',(65.4347826086958,173.041293409847,80.));
#20028=CARTESIAN_POINT('Ctrl Pts',(66.6461323784681,172.404050954516,80.));
#20029=CARTESIAN_POINT('Ctrl Pts',(67.8488741821648,171.755204325261,79.9919611843668));
#20030=CARTESIAN_POINT('Ctrl Pts',(69.0430590209991,171.094827191335,79.9763199823015));
#20031=CARTESIAN_POINT('Ctrl Pts',(70.2450844944289,170.430114232975,79.9605760851207));
#20032=CARTESIAN_POINT('Ctrl Pts',(71.4384404980377,169.753719199296,79.9371296605925));
#20033=CARTESIAN_POINT('Ctrl Pts',(72.6232020546047,169.065715093842,79.9063781002701));
#20034=CARTESIAN_POINT('Ctrl Pts',(73.8175810187664,168.372126053704,79.8753769114143));
#20035=CARTESIAN_POINT('Ctrl Pts',(75.0032256809894,167.666739016059,79.8369515176592));
#20036=CARTESIAN_POINT('Ctrl Pts',(76.1802326477079,166.949621683208,79.7914605218376));
#20037=CARTESIAN_POINT('Ctrl Pts',(76.5129016171382,166.746935810629,79.7786029575867));
#20038=CARTESIAN_POINT('Ctrl Pts',(76.8448806696896,166.543312801713,79.7651806603313));
#20039=CARTESIAN_POINT('Ctrl Pts',(77.1761722268184,166.338754031917,79.7512010309385));
#20040=CARTESIAN_POINT('Ctrl Pts',(78.4502335131952,165.552074130852,79.6974390070534));
#20041=CARTESIAN_POINT('Ctrl Pts',(79.7141132075376,164.751552111255,79.6354392698203));
#20042=CARTESIAN_POINT('Ctrl Pts',(80.967841633028,163.937227172555,79.5656043347192));
#20043=CARTESIAN_POINT('Ctrl Pts',(82.2296315257554,163.117666128747,79.4953203613495));
#20044=CARTESIAN_POINT('Ctrl Pts',(83.4811394894385,162.284124393098,79.4171000956569));
#20045=CARTESIAN_POINT('Ctrl Pts',(84.7224110600106,161.436629785652,79.3313044021991));
#20046=CARTESIAN_POINT('Ctrl Pts',(85.9469000979227,160.600593674691,79.2466687039122));
#20047=CARTESIAN_POINT('Ctrl Pts',(87.1614280078243,159.750979641084,79.1546608597167));
#20048=CARTESIAN_POINT('Ctrl Pts',(88.3660478508558,158.887798928392,79.0555809796938));
#20049=CARTESIAN_POINT('Ctrl Pts',(89.6734044670519,157.951001296975,78.9480510087828));
#20050=CARTESIAN_POINT('Ctrl Pts',(90.9690817922079,156.998223705516,78.8321926827009));
#20051=CARTESIAN_POINT('Ctrl Pts',(92.2530681368108,156.0294369149,78.7083568595487));
#20052=CARTESIAN_POINT('Ctrl Pts',(93.5372691533739,155.060488151098,78.584500332065));
#20053=CARTESIAN_POINT('Ctrl Pts',(94.8097756557245,154.075525043431,78.4526635519813));
#20054=CARTESIAN_POINT('Ctrl Pts',(96.0705771572415,153.074497779078,78.3131497015861));
#20055=CARTESIAN_POINT('Ctrl Pts',(97.058088528114,152.290452229549,78.2038767403042));
#20056=CARTESIAN_POINT('Ctrl Pts',(98.0384193587957,151.496551473984,78.0898931912743));
#20057=CARTESIAN_POINT('Ctrl Pts',(99.0115628561522,150.692761639502,77.9713247989972));
#20058=CARTESIAN_POINT('Ctrl Pts',(100.294220382482,149.633321707378,77.8150450302352));
#20059=CARTESIAN_POINT('Ctrl Pts',(101.564380068726,148.556699124926,77.6508055324762));
#20060=CARTESIAN_POINT('Ctrl Pts',(102.821978092576,147.462776792109,77.4788690746293));
#20061=CARTESIAN_POINT('Ctrl Pts',(103.259527029588,147.082174608566,77.4190481994867));
#20062=CARTESIAN_POINT('Ctrl Pts',(103.695555249051,146.69947804494,77.3582952087644));
#20063=CARTESIAN_POINT('Ctrl Pts',(104.130059658361,146.314681445384,77.2966199393637));
#20064=CARTESIAN_POINT('Ctrl Pts',(104.971735602031,145.569294208538,77.1771491366246));
#20065=CARTESIAN_POINT('Ctrl Pts',(105.806692611071,144.816904703943,77.0543582486579));
#20066=CARTESIAN_POINT('Ctrl Pts',(106.634220566184,144.058207403801,76.9284556400773));
#20067=CARTESIAN_POINT('Ctrl Pts',(107.461748521298,143.299510103659,76.8025530314967));
#20068=CARTESIAN_POINT('Ctrl Pts',(108.281847257875,142.534505115263,76.6735387741947));
#20069=CARTESIAN_POINT('Ctrl Pts',(109.093843490683,141.763932442456,76.5416368750921));
#20070=CARTESIAN_POINT('Ctrl Pts',(110.282654488823,140.635768011038,76.3485246142302));
#20071=CARTESIAN_POINT('Ctrl Pts',(111.455138482761,139.494739173689,76.1490506803267));
#20072=CARTESIAN_POINT('Ctrl Pts',(112.611420646104,138.340968291007,75.9435279501095));
#20073=CARTESIAN_POINT('Ctrl Pts',(113.769896451987,137.185008530064,75.7376153121186));
#20074=CARTESIAN_POINT('Ctrl Pts',(114.912109249862,136.016258399039,75.5256307997759));
#20075=CARTESIAN_POINT('Ctrl Pts',(116.038181686695,134.834807735391,75.307848804401));
#20076=CARTESIAN_POINT('Ctrl Pts',(117.166182792069,133.651333554735,75.0896938052392));
#20077=CARTESIAN_POINT('Ctrl Pts',(118.277988553096,132.455115332012,74.8657213326374));
#20078=CARTESIAN_POINT('Ctrl Pts',(119.373713676575,131.246209304145,74.636168474289));
#20079=CARTESIAN_POINT('Ctrl Pts',(120.46960611424,130.037118679682,74.406580563856));
#20080=CARTESIAN_POINT('Ctrl Pts',(121.549413346339,128.815336367242,74.1714104337045));
#20081=CARTESIAN_POINT('Ctrl Pts',(122.613236345249,127.580884409607,73.9308584323559));
#20082=CARTESIAN_POINT('Ctrl Pts',(123.676359826661,126.347244166651,73.6904646061305));
#20083=CARTESIAN_POINT('Ctrl Pts',(124.723520420591,125.100950892824,73.444695846114));
#20084=CARTESIAN_POINT('Ctrl Pts',(125.75480007494,123.841992797908,73.1937173237016));
#20085=CARTESIAN_POINT('Ctrl Pts',(126.219366288216,123.274863026308,73.0806576494622));
#20086=CARTESIAN_POINT('Ctrl Pts',(126.680709527289,122.705162753967,72.966540311257));
#20087=CARTESIAN_POINT('Ctrl Pts',(127.138835761371,122.13288870443,72.8513782152747));
#20088=CARTESIAN_POINT('Ctrl Pts',(128.210661006918,120.794004946999,72.5819467079277));
#20089=CARTESIAN_POINT('Ctrl Pts',(129.264832288659,119.441061318821,72.3068215265784));
#20090=CARTESIAN_POINT('Ctrl Pts',(130.301341770802,118.074024048082,72.0261836067221));
#20091=CARTESIAN_POINT('Ctrl Pts',(131.333339219409,116.712937632707,71.7467673329075));
#20092=CARTESIAN_POINT('Ctrl Pts',(132.347828610888,115.337879883744,71.461886051324));
#20093=CARTESIAN_POINT('Ctrl Pts',(133.344772650024,113.948787359142,71.171688683276));
#20094=CARTESIAN_POINT('Ctrl Pts',(133.934200329062,113.127507978754,71.0001139966372));
#20095=CARTESIAN_POINT('Ctrl Pts',(134.517494302768,112.30132206452,70.8266804775351));
#20096=CARTESIAN_POINT('Ctrl Pts',(135.094641307937,111.470211814142,70.6514143384368));
#20097=CARTESIAN_POINT('Ctrl Pts',(135.728081448236,110.558037638606,70.4590532818156));
#20098=CARTESIAN_POINT('Ctrl Pts',(136.354463262642,109.639420272454,70.2643779700071));
#20099=CARTESIAN_POINT('Ctrl Pts',(136.97318350466,108.715168561764,70.067597497168));
#20100=CARTESIAN_POINT('Ctrl Pts',(137.591903746677,107.790916851074,69.8708170243288));
#20101=CARTESIAN_POINT('Ctrl Pts',(138.20296226777,106.861030923092,69.6719314547462));
#20102=CARTESIAN_POINT('Ctrl Pts',(138.805802472581,105.926356872724,69.4711632769561));
#20103=CARTESIAN_POINT('Ctrl Pts',(139.686395610747,104.561040577283,69.1778930565674));
#20104=CARTESIAN_POINT('Ctrl Pts',(140.548033055148,103.18773742639,68.8810855487316));
#20105=CARTESIAN_POINT('Ctrl Pts',(141.39095234604,101.806527636459,68.5809000334162));
#20106=CARTESIAN_POINT('Ctrl Pts',(141.702131618801,101.29662845322,68.4700809889848));
#20107=CARTESIAN_POINT('Ctrl Pts',(142.010759658666,100.785651337718,68.358801298185));
#20108=CARTESIAN_POINT('Ctrl Pts',(142.316847597481,100.273599037248,68.2470680358434));
#20109=CARTESIAN_POINT('Ctrl Pts',(143.188689922049,98.8151003140736,67.9288137865961));
#20110=CARTESIAN_POINT('Ctrl Pts',(144.039953118992,97.3478506960236,67.6068657481795));
#20111=CARTESIAN_POINT('Ctrl Pts',(144.870820280825,95.8719469048255,67.2813968647469));
#20112=CARTESIAN_POINT('Ctrl Pts',(145.744966077093,94.3191654807479,66.9389747913547));
#20113=CARTESIAN_POINT('Ctrl Pts',(146.596536296559,92.7568049920601,66.5926556152579));
#20114=CARTESIAN_POINT('Ctrl Pts',(147.425710892994,91.1849357183585,66.242609978645));
#20115=CARTESIAN_POINT('Ctrl Pts',(148.217312758539,89.6842932061474,65.9084261045126));
#20116=CARTESIAN_POINT('Ctrl Pts',(148.988502674307,88.1749836666552,65.5708454866793));
#20117=CARTESIAN_POINT('Ctrl Pts',(149.739404058878,86.6570340611208,65.2299920279374));
#20118=CARTESIAN_POINT('Ctrl Pts',(150.490623793833,85.1384409092449,64.8889940617655));
#20119=CARTESIAN_POINT('Ctrl Pts',(151.221538035357,83.6112001634024,64.5447203357147));
#20120=CARTESIAN_POINT('Ctrl Pts',(151.932234113087,82.0753083209362,64.197273065751));
#20121=CARTESIAN_POINT('Ctrl Pts',(152.642725551019,80.5398587274236,63.8499258407172));
#20122=CARTESIAN_POINT('Ctrl Pts',(153.333010691149,78.9957627989489,63.4994067527238));
#20123=CARTESIAN_POINT('Ctrl Pts',(154.003137062145,77.4429897178712,63.145798278425));
#20124=CARTESIAN_POINT('Ctrl Pts',(154.098169966934,77.2227856746341,63.0956518554142));
#20125=CARTESIAN_POINT('Ctrl Pts',(154.192797389382,77.0024070831775,63.0454432714742));
#20126=CARTESIAN_POINT('Ctrl Pts',(154.287019396353,76.7818538151815,62.995172732479));
#20127=CARTESIAN_POINT('Ctrl Pts',(154.969920185579,75.1833312871433,62.6308227057908));
#20128=CARTESIAN_POINT('Ctrl Pts',(155.631509575676,73.5756648494386,62.2632351988744));
#20129=CARTESIAN_POINT('Ctrl Pts',(156.271767918129,71.9588255780039,61.8925027191992));
#20130=CARTESIAN_POINT('Ctrl Pts',(156.90994347294,70.3472459535393,61.5229762480604));
#20131=CARTESIAN_POINT('Ctrl Pts',(157.52692671005,68.7265528117573,61.1503250777792));
#20132=CARTESIAN_POINT('Ctrl Pts',(158.122652620036,67.0966980818089,60.774625906449));
#20133=CARTESIAN_POINT('Ctrl Pts',(158.436687411552,66.2375259663423,60.5765774264958));
#20134=CARTESIAN_POINT('Ctrl Pts',(158.744814366495,65.3758076965917,60.3776817221769));
#20135=CARTESIAN_POINT('Ctrl Pts',(159.047018599036,64.5115344360402,60.1779485747607));
#20136=CARTESIAN_POINT('Ctrl Pts',(159.616169765598,62.8838201901668,59.8017845717057));
#20137=CARTESIAN_POINT('Ctrl Pts',(160.164315738842,61.2470442552432,59.4226520428314));
#20138=CARTESIAN_POINT('Ctrl Pts',(160.691320701882,59.6011287064151,59.0406108572493));
#20139=CARTESIAN_POINT('Ctrl Pts',(160.835925898711,59.1495049863498,58.9357823552198));
#20140=CARTESIAN_POINT('Ctrl Pts',(160.978939094884,58.6971930807887,58.8307348028855));
#20141=CARTESIAN_POINT('Ctrl Pts',(161.12035681976,58.2441912509891,58.7254693140811));
#20142=CARTESIAN_POINT('Ctrl Pts',(161.390759200204,57.3780143044214,58.5241929975773));
#20143=CARTESIAN_POINT('Ctrl Pts',(161.65536766827,56.5091739433876,58.3220873619862));
#20144=CARTESIAN_POINT('Ctrl Pts',(161.913876783448,55.6386225203367,58.1193844025833));
#20145=CARTESIAN_POINT('Ctrl Pts',(162.172378437343,54.7680962237895,57.9166872937441));
#20146=CARTESIAN_POINT('Ctrl Pts',(162.424781040467,53.8958590880924,57.7133929440505));
#20147=CARTESIAN_POINT('Ctrl Pts',(162.6708283902,53.0228796342858,57.5097391548275));
#20148=CARTESIAN_POINT('Ctrl Pts',(162.776391719317,52.6483394594182,57.4223642166254));
#20149=CARTESIAN_POINT('Ctrl Pts',(162.880785841691,52.2736628366288,57.3349231841326));
#20150=CARTESIAN_POINT('Ctrl Pts',(162.983993330494,51.898927081956,57.2474351316884));
#20151=CARTESIAN_POINT('Ctrl Pts',(163.44181462992,50.236625129495,56.8593441673714));
#20152=CARTESIAN_POINT('Ctrl Pts',(163.876849494941,48.5711473098526,56.4698531943719));
#20153=CARTESIAN_POINT('Ctrl Pts',(164.289304748925,46.9025389459629,56.0790556533708));
#20154=CARTESIAN_POINT('Ctrl Pts',(164.712616410982,45.1900104401014,55.6779717660619));
#20155=CARTESIAN_POINT('Ctrl Pts',(165.112144521505,43.4741842389034,55.2755115308422));
#20156=CARTESIAN_POINT('Ctrl Pts',(165.488065228237,41.7550820886685,54.8717608318544));
#20157=CARTESIAN_POINT('Ctrl Pts',(165.856698167564,40.06930722366,54.4758374249816));
#20158=CARTESIAN_POINT('Ctrl Pts',(166.2026301339,38.3803818300019,54.078672912382));
#20159=CARTESIAN_POINT('Ctrl Pts',(166.525980271794,36.688304964299,53.6803362266353));
#20160=CARTESIAN_POINT('Ctrl Pts',(166.858919218813,34.9460502876389,53.2701870379699));
#20161=CARTESIAN_POINT('Ctrl Pts',(167.167917546405,33.2004542212604,52.8587950132626));
#20162=CARTESIAN_POINT('Ctrl Pts',(167.453051830328,31.4514970984036,52.4462246664667));
#20163=CARTESIAN_POINT('Ctrl Pts',(167.738186114251,29.7025399755469,52.0336543196709));
#20164=CARTESIAN_POINT('Ctrl Pts',(167.999456457707,27.9502214508155,51.6199054808393));
#20165=CARTESIAN_POINT('Ctrl Pts',(168.236883475619,26.1945080380638,51.2050343015782));
#20166=CARTESIAN_POINT('Ctrl Pts',(168.470502966904,24.4669503323876,50.7968162533534));
#20167=CARTESIAN_POINT('Ctrl Pts',(168.681033417607,22.7361302648766,50.3875209152059));
#20168=CARTESIAN_POINT('Ctrl Pts',(168.86844066887,21.0020257404361,49.9772058899181));
#20169=CARTESIAN_POINT('Ctrl Pts',(169.055408494949,19.2719872763818,49.5678529552349));
#20170=CARTESIAN_POINT('Ctrl Pts',(169.21936146439,17.5386794258596,49.1574849600718));
#20171=CARTESIAN_POINT('Ctrl Pts',(169.360214013948,15.8020771827112,48.7461560842687));
#20172=CARTESIAN_POINT('Ctrl Pts',(169.431623414445,14.9216548866687,48.537620644048));
#20173=CARTESIAN_POINT('Ctrl Pts',(169.497094521659,14.0403858180888,48.328838195924));
#20174=CARTESIAN_POINT('Ctrl Pts',(169.556611063575,13.1582668116683,48.1198156901436));
#20175=CARTESIAN_POINT('Ctrl Pts',(169.672434204295,11.4416046783918,47.7130440209424));
#20176=CARTESIAN_POINT('Ctrl Pts',(169.765709655592,9.72172177919562,47.3053630211217));
#20177=CARTESIAN_POINT('Ctrl Pts',(169.836279969576,7.99858073586123,46.8968207381216));
#20178=CARTESIAN_POINT('Ctrl Pts',(169.855452850521,7.5304295231175,46.7858260137005));
#20179=CARTESIAN_POINT('Ctrl Pts',(169.872949511331,7.06203785414009,46.6747677241711));
#20180=CARTESIAN_POINT('Ctrl Pts',(169.888766135311,6.59340507295846,46.5636468581297));
#20181=CARTESIAN_POINT('Ctrl Pts',(169.9257828563,5.49663189754684,46.3035831366046));
#20182=CARTESIAN_POINT('Ctrl Pts',(169.953598091479,4.39853740250482,46.0431764899174));
#20183=CARTESIAN_POINT('Ctrl Pts',(169.972156850062,3.29911036932559,45.782438961203));
#20184=CARTESIAN_POINT('Ctrl Pts',(169.981436229354,2.74939685273598,45.6520701968457));
#20185=CARTESIAN_POINT('Ctrl Pts',(169.988401335714,2.19927120329341,45.5215999770967));
#20186=CARTESIAN_POINT('Ctrl Pts',(169.993042478652,1.64921227805479,45.3911437233179));
#20187=CARTESIAN_POINT('Ctrl Pts',(169.995363050121,1.37418281543549,45.3259155964285));
#20188=CARTESIAN_POINT('Ctrl Pts',(169.997103130708,1.09914979647015,45.2606861617961));
#20189=CARTESIAN_POINT('Ctrl Pts',(169.998262721974,0.824113169007625,45.1954556393542));
#20190=CARTESIAN_POINT('Ctrl Pts',(169.999310371452,0.575627355555245,45.1365221817255));
#20191=CARTESIAN_POINT('Ctrl Pts',(169.999884019389,0.326147221333698,45.0773527091105));
#20192=CARTESIAN_POINT('Ctrl Pts',(169.999983994202,0.0791027940534806,
45.0187609002855));
#20193=CARTESIAN_POINT('Ctrl Pts',(169.999994676552,0.0527059927639873,
45.0125003407911));
#20194=CARTESIAN_POINT('Ctrl Pts',(170.,0.0263369999825807,45.0062463764957));
#20195=CARTESIAN_POINT('Ctrl Pts',(170.,3.49024337756996E-14,45.));
#20196=CARTESIAN_POINT('Ctrl Pts',(65.4171737766276,173.051051117154,79.9999995059578));
#20197=CARTESIAN_POINT('Ctrl Pts',(60.1122246678144,159.017358945106,79.9970990772669));
#20198=CARTESIAN_POINT('Ctrl Pts',(60.1111292806026,159.017773023373,94.9999991814784));
#20199=CARTESIAN_POINT('Ctrl Pts',(69.4980654230037,170.904781366711,80.0002461066156));
#20200=CARTESIAN_POINT('Ctrl Pts',(63.9530125618426,157.565452095818,80.5517562050311));
#20201=CARTESIAN_POINT('Ctrl Pts',(64.2759055369405,157.443423435057,95.0003752334648));
#20202=CARTESIAN_POINT('Ctrl Pts',(73.4707404887855,168.632425582207,79.9097827742579));
#20203=CARTESIAN_POINT('Ctrl Pts',(67.8395215153769,155.937211445011,80.9562032488646));
#20204=CARTESIAN_POINT('Ctrl Pts',(68.3475774635587,155.717622842009,94.8711639053697));
#20205=CARTESIAN_POINT('Ctrl Pts',(81.2094588046944,163.843390610061,79.5786121468522));
#20206=CARTESIAN_POINT('Ctrl Pts',(75.4920654363854,152.377267497421,81.4803629792958));
#20207=CARTESIAN_POINT('Ctrl Pts',(76.3074783717929,151.97526765444,94.3981030531638));
#20208=CARTESIAN_POINT('Ctrl Pts',(84.9757899122008,161.327031171744,79.3379637809786));
#20209=CARTESIAN_POINT('Ctrl Pts',(79.2729405826562,150.450643097299,81.6101590419467));
#20210=CARTESIAN_POINT('Ctrl Pts',(80.1959679691824,149.959099180759,94.0543379213307));
#20211=CARTESIAN_POINT('Ctrl Pts',(92.3178906398677,156.046341834353,78.726584215355));
#20212=CARTESIAN_POINT('Ctrl Pts',(86.703867958156,146.292589569395,81.6312588050202));
#20213=CARTESIAN_POINT('Ctrl Pts',(87.8000684551384,145.63747005799,93.1809712877857));
#20214=CARTESIAN_POINT('Ctrl Pts',(95.8936351170506,153.282013829614,78.3557679502871));
#20215=CARTESIAN_POINT('Ctrl Pts',(90.366568547758,144.064645410308,81.5291707439827));
#20216=CARTESIAN_POINT('Ctrl Pts',(91.5156662167517,143.332003833601,92.6512484049633));
#20217=CARTESIAN_POINT('Ctrl Pts',(101.118204191116,148.945321347681,77.7118506792732));
#20218=CARTESIAN_POINT('Ctrl Pts',(95.7862627827622,140.469122843766,81.2184413297099));
#20219=CARTESIAN_POINT('Ctrl Pts',(96.9597420465698,139.655302598131,91.7313856490923));
#20220=CARTESIAN_POINT('Ctrl Pts',(102.836519125185,147.468018930124,77.482549849181));
#20221=CARTESIAN_POINT('Ctrl Pts',(97.565644447969,139.240074537784,81.090445307719));
#20222=CARTESIAN_POINT('Ctrl Pts',(98.7528522876237,138.393276733981,91.4038190221291));
#20223=CARTESIAN_POINT('Ctrl Pts',(106.226989159944,144.448761853408,76.995800971589));
#20224=CARTESIAN_POINT('Ctrl Pts',(101.08836341206,136.704210075211,80.7859435362935));
#20225=CARTESIAN_POINT('Ctrl Pts',(102.295631429104,135.795539951172,90.7084745843325));
#20226=CARTESIAN_POINT('Ctrl Pts',(107.890968873499,142.914010809927,76.7395043574806));
#20227=CARTESIAN_POINT('Ctrl Pts',(102.824700615765,135.403548235755,80.6106070677653));
#20228=CARTESIAN_POINT('Ctrl Pts',(104.036759724697,134.466015015203,90.3423416598691));
#20229=CARTESIAN_POINT('Ctrl Pts',(112.780952654854,138.245372609845,75.9362630272676));
#20230=CARTESIAN_POINT('Ctrl Pts',(107.914041409476,131.435704892851,80.0241711268571));
#20231=CARTESIAN_POINT('Ctrl Pts',(109.159801879539,130.396180641736,89.194868194963));
#20232=CARTESIAN_POINT('Ctrl Pts',(115.910241252279,135.042722467798,75.3543730521059));
#20233=CARTESIAN_POINT('Ctrl Pts',(111.217729890296,128.654798675575,79.5479025767146));
#20234=CARTESIAN_POINT('Ctrl Pts',(112.446820922398,127.570888947572,88.3636043218873));
#20235=CARTESIAN_POINT('Ctrl Pts',(121.921081660961,128.457279192248,74.1087295936706));
#20236=CARTESIAN_POINT('Ctrl Pts',(117.585782041987,122.859192470861,78.4483848144859));
#20237=CARTESIAN_POINT('Ctrl Pts',(118.773955284971,121.701958851907,86.5841254177092));
#20238=CARTESIAN_POINT('Ctrl Pts',(124.802595831012,125.07448269568,73.4449368880087));
#20239=CARTESIAN_POINT('Ctrl Pts',(120.661020346731,119.8431662431,77.8267940081951));
#20240=CARTESIAN_POINT('Ctrl Pts',(121.814041889375,118.658306100492,85.6358543716459));
#20241=CARTESIAN_POINT('Ctrl Pts',(130.325562286974,118.125822190644,72.0427084253293));
#20242=CARTESIAN_POINT('Ctrl Pts',(126.571701806773,113.57987068343,76.4540968289114));
#20243=CARTESIAN_POINT('Ctrl Pts',(127.651676978702,112.354366949351,83.6326763250335));
#20244=CARTESIAN_POINT('Ctrl Pts',(132.966997982629,114.559964739603,71.3042501994499));
#20245=CARTESIAN_POINT('Ctrl Pts',(129.416365550538,110.330915246744,75.7039088018499));
#20246=CARTESIAN_POINT('Ctrl Pts',(130.449215516202,109.094078884113,82.5777372261749));
#20247=CARTESIAN_POINT('Ctrl Pts',(136.120374389438,109.984367133449,70.3373592580949));
#20248=CARTESIAN_POINT('Ctrl Pts',(132.838493553414,106.101344893951,74.6872762465277));
#20249=CARTESIAN_POINT('Ctrl Pts',(133.794311682361,104.88202612324,81.1964639412465));
#20250=CARTESIAN_POINT('Ctrl Pts',(136.743616942198,109.063325258521,70.1417843056297));
#20251=CARTESIAN_POINT('Ctrl Pts',(133.511839276197,105.252753785792,74.4814177447014));
#20252=CARTESIAN_POINT('Ctrl Pts',(134.455728161604,104.03277160558,80.9170710194299));
#20253=CARTESIAN_POINT('Ctrl Pts',(137.975229697851,107.209266309907,69.7462901240218));
#20254=CARTESIAN_POINT('Ctrl Pts',(134.843563811306,103.540882689278,74.0625229474022));
#20255=CARTESIAN_POINT('Ctrl Pts',(135.763304172514,102.320504511889,80.3520788936533));
#20256=CARTESIAN_POINT('Ctrl Pts',(138.584011129024,106.275579631437,69.5462255028335));
#20257=CARTESIAN_POINT('Ctrl Pts',(135.502515209047,102.676936655468,73.8493312382261));
#20258=CARTESIAN_POINT('Ctrl Pts',(136.409901038821,101.456869632069,80.0662719859412));
#20259=CARTESIAN_POINT('Ctrl Pts',(140.381410996897,103.46681038063,68.9418375941936));
#20260=CARTESIAN_POINT('Ctrl Pts',(137.44622664547,100.0771502473,73.2027293733177));
#20261=CARTESIAN_POINT('Ctrl Pts',(138.319688906568,98.8549121117867,79.202859577207));
#20262=CARTESIAN_POINT('Ctrl Pts',(141.543035442275,101.581203701731,68.5327283633642));
#20263=CARTESIAN_POINT('Ctrl Pts',(138.70739707142,98.3214899215068,72.7594318660626));
#20264=CARTESIAN_POINT('Ctrl Pts',(139.554945257313,97.1029464009744,78.6184167041338));
#20265=CARTESIAN_POINT('Ctrl Pts',(147.172811063143,92.087379772777,66.4580230839566));
#20266=CARTESIAN_POINT('Ctrl Pts',(144.769209540695,89.533625084567,70.5112314665258));
#20267=CARTESIAN_POINT('Ctrl Pts',(145.545768022766,88.2579658671962,75.6545459907609));
#20268=CARTESIAN_POINT('Ctrl Pts',(151.109449633708,84.2828338416036,64.7059125945462));
#20269=CARTESIAN_POINT('Ctrl Pts',(149.105656521244,82.1186746640789,68.5241447463077));
#20270=CARTESIAN_POINT('Ctrl Pts',(149.748394838999,80.9109007293675,73.1515201292455));
#20271=CARTESIAN_POINT('Ctrl Pts',(156.211187639656,72.2434629872912,61.9599182770527));
#20272=CARTESIAN_POINT('Ctrl Pts',(154.735913992316,70.5418248837457,65.3361267841599));
#20273=CARTESIAN_POINT('Ctrl Pts',(155.204094851699,69.494444703793,69.2286486643273));
#20274=CARTESIAN_POINT('Ctrl Pts',(157.777199757704,68.1747130608376,61.0247584570915));
#20275=CARTESIAN_POINT('Ctrl Pts',(156.462811523132,66.6261512273264,64.2443587388644));
#20276=CARTESIAN_POINT('Ctrl Pts',(156.880610977599,65.6227064854861,67.8926978274835));
#20277=CARTESIAN_POINT('Ctrl Pts',(159.924440854169,61.9838631433058,59.5934387075325));
#20278=CARTESIAN_POINT('Ctrl Pts',(158.835393854645,60.637084725701,62.5584808456691));
#20279=CARTESIAN_POINT('Ctrl Pts',(159.181124815158,59.7146207337651,65.8479415995783));
#20280=CARTESIAN_POINT('Ctrl Pts',(160.606519612154,59.9056105043635,59.1115603052182));
#20281=CARTESIAN_POINT('Ctrl Pts',(159.588605202354,58.6261359817312,61.9898219519289));
#20282=CARTESIAN_POINT('Ctrl Pts',(159.91221396583,57.7284955929032,65.1595391420191));
#20283=CARTESIAN_POINT('Ctrl Pts',(161.578790554131,56.7655952183065,58.381658570037));
#20284=CARTESIAN_POINT('Ctrl Pts',(160.663581107371,55.5804420707533,61.1251183623648));
#20285=CARTESIAN_POINT('Ctrl Pts',(160.954720457782,54.7238687144436,64.1168149427384));
#20286=CARTESIAN_POINT('Ctrl Pts',(161.894669322878,55.7142130958785,58.1369583834399));
#20287=CARTESIAN_POINT('Ctrl Pts',(161.012707510978,54.5605741948746,60.8350012341958));
#20288=CARTESIAN_POINT('Ctrl Pts',(161.293483687908,53.7171877677032,63.7672407289973));
#20289=CARTESIAN_POINT('Ctrl Pts',(162.507622034656,53.609926721994,57.6466368798811));
#20290=CARTESIAN_POINT('Ctrl Pts',(161.690355249542,52.5177903875452,60.2528453586207));
#20291=CARTESIAN_POINT('Ctrl Pts',(161.950956676584,51.7011776789588,63.0667763221949));
#20292=CARTESIAN_POINT('Ctrl Pts',(162.804784056278,52.5568039701366,57.4009654066192));
#20293=CARTESIAN_POINT('Ctrl Pts',(162.019036836798,51.4945755320385,59.9607244749972));
#20294=CARTESIAN_POINT('Ctrl Pts',(162.269760743604,50.6916407802224,62.7158144755576));
#20295=CARTESIAN_POINT('Ctrl Pts',(165.396228192944,43.0696062215838,55.1854558190958));
#20296=CARTESIAN_POINT('Ctrl Pts',(164.871359483185,42.3174710775594,57.3363962613807));
#20297=CARTESIAN_POINT('Ctrl Pts',(165.050384666089,41.5921040022264,59.5507777172448));
#20298=CARTESIAN_POINT('Ctrl Pts',(167.112953991422,34.5721559152113,53.1846925294639));
#20299=CARTESIAN_POINT('Ctrl Pts',(166.788260728433,33.9828141288519,54.9228163985495));
#20300=CARTESIAN_POINT('Ctrl Pts',(166.895487919238,33.4066584126088,56.6925206006809));
#20301=CARTESIAN_POINT('Ctrl Pts',(168.839541545282,21.7037023432943,50.1437575021141));
#20302=CARTESIAN_POINT('Ctrl Pts',(168.70884062626,21.342590484654,51.2420487378816));
#20303=CARTESIAN_POINT('Ctrl Pts',(168.751767516685,20.9849502863122,52.3482901787236));
#20304=CARTESIAN_POINT('Ctrl Pts',(169.272994226546,17.3937906477954,49.123418475587));
#20305=CARTESIAN_POINT('Ctrl Pts',(169.191375205164,17.10625282417,50.0050582261906));
#20306=CARTESIAN_POINT('Ctrl Pts',(169.217967102382,16.8203670207432,50.8906501976363));
#20307=CARTESIAN_POINT('Ctrl Pts',(169.708244737431,10.8943962228678,47.5833483445016));
#20308=CARTESIAN_POINT('Ctrl Pts',(169.675477965546,10.7154189680991,48.1364420790708));
#20309=CARTESIAN_POINT('Ctrl Pts',(169.686138855143,10.5368669288742,48.690530528023));
#20310=CARTESIAN_POINT('Ctrl Pts',(169.817467420501,8.72217091897812,47.0683956196518));
#20311=CARTESIAN_POINT('Ctrl Pts',(169.796983990652,8.5791113628161,47.5113888393872));
#20312=CARTESIAN_POINT('Ctrl Pts',(169.803634766948,8.43625666941946,47.9548772375799));
#20313=CARTESIAN_POINT('Ctrl Pts',(169.963400726732,4.36546597417207,46.0353525704263));
#20314=CARTESIAN_POINT('Ctrl Pts',(169.959277929682,4.29443906431818,46.2573336219265));
#20315=CARTESIAN_POINT('Ctrl Pts',(169.960625243948,4.22263819734908,46.4790883103916));
#20316=CARTESIAN_POINT('Ctrl Pts',(170.,2.17934967149295,45.5168739027144));
#20317=CARTESIAN_POINT('Ctrl Pts',(170.,2.14369814666887,45.6276358938455));
#20318=CARTESIAN_POINT('Ctrl Pts',(170.,2.10804680089195,45.7383979484285));
#20319=CARTESIAN_POINT('Ctrl Pts',(170.,0.,45.));
#20320=CARTESIAN_POINT('Ctrl Pts',(170.,0.,45.));
#20321=CARTESIAN_POINT('Ctrl Pts',(170.,0.,45.));
#20322=CARTESIAN_POINT('Origin',(65.4347826086958,173.041293409847,95.));
#20323=CARTESIAN_POINT('Origin',(0.,0.,95.));
#20324=CARTESIAN_POINT('Origin',(-14.5652173913043,184.425742352699,95.));
#20325=CARTESIAN_POINT('Ctrl Pts',(-13.3842538190363,169.472303783561,95.));
#20326=CARTESIAN_POINT('Ctrl Pts',(-13.3842538190363,169.472303783561,80.));
#20327=CARTESIAN_POINT('Ctrl Pts',(-14.5652173913043,184.425742352699,80.));
#20328=CARTESIAN_POINT('Ctrl Pts',(-17.5395512351767,169.144134790342,95.));
#20329=CARTESIAN_POINT('Ctrl Pts',(-17.2144232870799,169.169812112664,79.3644410713064));
#20330=CARTESIAN_POINT('Ctrl Pts',(-18.7318660089282,184.721037013812,80.));
#20331=CARTESIAN_POINT('Ctrl Pts',(-21.6441982168127,168.666370511884,94.8172074050833));
#20332=CARTESIAN_POINT('Ctrl Pts',(-20.8543660593525,168.752921516777,78.5305161733615));
#20333=CARTESIAN_POINT('Ctrl Pts',(-22.876822841872,184.876406726332,79.8720451835484));
#20334=CARTESIAN_POINT('Ctrl Pts',(-29.7513824612582,167.426614072389,94.060173223671));
#20335=CARTESIAN_POINT('Ctrl Pts',(-27.8670083443154,167.750643110992,76.4491424798736));
#20336=CARTESIAN_POINT('Ctrl Pts',(-31.1273096488505,184.919419561866,79.3421212565797));
#20337=CARTESIAN_POINT('Ctrl Pts',(-33.7540169272061,166.664538735009,93.4863288792126));
#20338=CARTESIAN_POINT('Ctrl Pts',(-31.2373560808963,167.15512258256,75.1777949173772));
#20339=CARTESIAN_POINT('Ctrl Pts',(-35.2329409933915,184.807006229873,78.9404302153998));
#20340=CARTESIAN_POINT('Ctrl Pts',(-39.6776586745835,165.317222135875,92.2879046923386));
#20341=CARTESIAN_POINT('Ctrl Pts',(-35.9693696574127,166.20324713768,72.9549331576006));
#20342=CARTESIAN_POINT('Ctrl Pts',(-41.3622144006103,184.443659034893,78.1015332846615));
#20343=CARTESIAN_POINT('Ctrl Pts',(-41.6387819418482,164.834067193048,91.8318643970813));
#20344=CARTESIAN_POINT('Ctrl Pts',(-37.5231338419952,165.868473328022,72.1406418324815));
#20345=CARTESIAN_POINT('Ctrl Pts',(-43.4004096859107,184.290063044221,77.7823050779236));
#20346=CARTESIAN_POINT('Ctrl Pts',(-44.5594044158236,164.059361041538,91.0538818796549));
#20347=CARTESIAN_POINT('Ctrl Pts',(-39.7599794861513,165.361699241537,70.8335077858203));
#20348=CARTESIAN_POINT('Ctrl Pts',(-46.4499795033957,184.011560356448,77.2377173157751));
#20349=CARTESIAN_POINT('Ctrl Pts',(-45.5294312692045,163.79279700543,90.7788716538768));
#20350=CARTESIAN_POINT('Ctrl Pts',(-40.4978371304263,165.190041788369,70.3778813312569));
#20351=CARTESIAN_POINT('Ctrl Pts',(-47.4652121610676,183.910707315012,77.0452101577021));
#20352=CARTESIAN_POINT('Ctrl Pts',(-47.4622527854103,163.243205136057,90.1955588967012));
#20353=CARTESIAN_POINT('Ctrl Pts',(-41.9450409744791,164.845993388777,69.4331574372367));
#20354=CARTESIAN_POINT('Ctrl Pts',(-49.4929835017655,183.693061788492,76.6368912277025));
#20355=CARTESIAN_POINT('Ctrl Pts',(-48.4266504515543,162.959685425406,89.8867032935461));
#20356=CARTESIAN_POINT('Ctrl Pts',(-42.6553053430736,164.673254829836,68.942551397809));
#20357=CARTESIAN_POINT('Ctrl Pts',(-50.5072136184811,183.576056117467,76.4206923054768));
#20358=CARTESIAN_POINT('Ctrl Pts',(-51.2966354956011,162.088412227551,88.9109268015102));
#20359=CARTESIAN_POINT('Ctrl Pts',(-44.7469464262981,164.155637506621,67.4128983527913));
#20360=CARTESIAN_POINT('Ctrl Pts',(-53.5329794899747,183.202867702932,75.7376487610681));
#20361=CARTESIAN_POINT('Ctrl Pts',(-53.1733448982289,161.481802427548,88.1971446848615));
#20362=CARTESIAN_POINT('Ctrl Pts',(-46.0494224580936,163.820664239566,66.3397922862081));
#20363=CARTESIAN_POINT('Ctrl Pts',(-55.5215816926986,182.925374134496,75.2380012793601));
#20364=CARTESIAN_POINT('Ctrl Pts',(-56.8511651327196,160.22397494123,86.6315720785634));
#20365=CARTESIAN_POINT('Ctrl Pts',(-48.478602658805,163.188342727077,64.082468778351));
#20366=CARTESIAN_POINT('Ctrl Pts',(-59.4384997234822,182.318483802645,74.1421004550374));
#20367=CARTESIAN_POINT('Ctrl Pts',(-58.6522951136164,159.572737982238,85.7798428475361));
#20368=CARTESIAN_POINT('Ctrl Pts',(-49.6000886182912,162.892055598081,62.8933190799086));
#20369=CARTESIAN_POINT('Ctrl Pts',(-61.3668401614234,181.989071709277,73.545889993238));
#20370=CARTESIAN_POINT('Ctrl Pts',(-62.1748189026221,158.23350569228,83.9219691980032));
#20371=CARTESIAN_POINT('Ctrl Pts',(-51.637017574247,162.366710734437,60.4121506921274));
#20372=CARTESIAN_POINT('Ctrl Pts',(-65.15798176608,181.284440720707,72.2453784386395));
#20373=CARTESIAN_POINT('Ctrl Pts',(-63.8962495517862,157.545478964947,82.9159377469876));
#20374=CARTESIAN_POINT('Ctrl Pts',(-52.545511584158,162.139981860392,59.1148834184348));
#20375=CARTESIAN_POINT('Ctrl Pts',(-67.0208288573461,180.909197594207,71.5411564228308));
#20376=CARTESIAN_POINT('Ctrl Pts',(-66.4135506755794,156.493026838041,81.2731565607321));
#20377=CARTESIAN_POINT('Ctrl Pts',(-53.7105373582531,161.881828084746,57.1273358583113));
#20378=CARTESIAN_POINT('Ctrl Pts',(-69.7596407351623,180.317443237727,70.3912095925427));
#20379=CARTESIAN_POINT('Ctrl Pts',(-67.2418202127918,156.138823420855,80.7032055873364));
#20380=CARTESIAN_POINT('Ctrl Pts',(-54.0699645553869,161.808931015126,56.4472226877468));
#20381=CARTESIAN_POINT('Ctrl Pts',(-70.6633063132461,180.115388269163,69.9922439111036));
#20382=CARTESIAN_POINT('Ctrl Pts',(-68.8754848173699,155.425101434584,79.514506063713));
#20383=CARTESIAN_POINT('Ctrl Pts',(-54.7189452269188,161.696107176842,55.0708260730923));
#20384=CARTESIAN_POINT('Ctrl Pts',(-72.4505873293311,179.702774329136,69.160154244631));
#20385=CARTESIAN_POINT('Ctrl Pts',(-69.6795919234263,155.066105739768,78.8965035406746));
#20386=CARTESIAN_POINT('Ctrl Pts',(-55.0063194658611,161.657075331116,54.3752022489627));
#20387=CARTESIAN_POINT('Ctrl Pts',(-73.3328070782591,179.492503237854,68.7275524784488));
#20388=CARTESIAN_POINT('Ctrl Pts',(-72.0324106623047,153.994488647569,76.9821802471142));
#20389=CARTESIAN_POINT('Ctrl Pts',(-55.7548099034461,161.598620210439,52.2723911996401));
#20390=CARTESIAN_POINT('Ctrl Pts',(-75.921231436318,178.857382701198,67.3875261730269));
#20391=CARTESIAN_POINT('Ctrl Pts',(-73.5292807993369,153.283865054872,75.62063975569));
#20392=CARTESIAN_POINT('Ctrl Pts',(-56.0781101307272,161.644219581938,50.8878411365529));
#20393=CARTESIAN_POINT('Ctrl Pts',(-77.5776030421959,178.426261084882,66.4344478289248));
#20394=CARTESIAN_POINT('Ctrl Pts',(-76.366751875532,151.890149874864,72.7006648710333));
#20395=CARTESIAN_POINT('Ctrl Pts',(-56.3756134497039,161.93051189576,48.2172467564738));
#20396=CARTESIAN_POINT('Ctrl Pts',(-80.7336339099764,177.564857597969,64.3904654097815));
#20397=CARTESIAN_POINT('Ctrl Pts',(-77.7075527077816,151.206919364782,71.1425408034194));
#20398=CARTESIAN_POINT('Ctrl Pts',(-56.3324815494095,162.180759006444,46.9371883104744));
#20399=CARTESIAN_POINT('Ctrl Pts',(-82.2335307362999,177.134474712401,63.2997785623094));
#20400=CARTESIAN_POINT('Ctrl Pts',(-79.5843975938565,150.222577239668,68.6265804660936));
#20401=CARTESIAN_POINT('Ctrl Pts',(-55.9936784211686,162.717602630982,45.2323932608695));
#20402=CARTESIAN_POINT('Ctrl Pts',(-84.3431679099447,176.505297510891,61.5386063263076));
#20403=CARTESIAN_POINT('Ctrl Pts',(-80.1887658265789,149.900578404234,67.755569241579));
#20404=CARTESIAN_POINT('Ctrl Pts',(-55.8294042116326,162.9288556975,44.6926349322782));
#20405=CARTESIAN_POINT('Ctrl Pts',(-85.0243102277581,176.297889106232,60.9288984690785));
#20406=CARTESIAN_POINT('Ctrl Pts',(-81.3314469036299,149.283680672992,65.9735353866643));
#20407=CARTESIAN_POINT('Ctrl Pts',(-55.4166431025694,163.399678588271,43.7235153888331));
#20408=CARTESIAN_POINT('Ctrl Pts',(-86.3151146859738,175.897970347453,59.6814747706918));
#20409=CARTESIAN_POINT('Ctrl Pts',(-81.871857983652,148.987704499459,65.0600083704848));
#20410=CARTESIAN_POINT('Ctrl Pts',(-55.1663164325277,163.660533878635,43.2952935416342));
#20411=CARTESIAN_POINT('Ctrl Pts',(-86.9271268382518,175.704778800986,59.0420058593072));
#20412=CARTESIAN_POINT('Ctrl Pts',(-82.8877983348762,148.424897200268,63.1847493041814));
#20413=CARTESIAN_POINT('Ctrl Pts',(-54.5968742872658,164.221510744674,42.5719496657066));
#20414=CARTESIAN_POINT('Ctrl Pts',(-88.0800512417677,175.335427624406,57.7293245129592));
#20415=CARTESIAN_POINT('Ctrl Pts',(-83.3633401165125,148.158058769467,62.2230271057914));
#20416=CARTESIAN_POINT('Ctrl Pts',(-54.276749072151,164.521983493455,42.2805814044158));
#20417=CARTESIAN_POINT('Ctrl Pts',(-88.6209776878574,175.159263160964,57.0561189740244));
#20418=CARTESIAN_POINT('Ctrl Pts',(-84.2452339637734,147.658380758111,60.2472126840058));
#20419=CARTESIAN_POINT('Ctrl Pts',(-53.5924579506749,165.144968110372,41.8573492354118));
#20420=CARTESIAN_POINT('Ctrl Pts',(-89.6259478489954,174.827893059694,55.6730488788336));
#20421=CARTESIAN_POINT('Ctrl Pts',(-84.6516057522163,147.425530224166,59.2331358058206));
#20422=CARTESIAN_POINT('Ctrl Pts',(-53.2282068700753,165.467180261645,41.7294386859836));
#20423=CARTESIAN_POINT('Ctrl Pts',(-90.0900138002506,174.672680323464,54.9631950640533));
#20424=CARTESIAN_POINT('Ctrl Pts',(-85.2047113619757,147.106092638268,57.668598294985));
#20425=CARTESIAN_POINT('Ctrl Pts',(-52.6783494190424,165.945140624608,41.6733190176321));
#20426=CARTESIAN_POINT('Ctrl Pts',(-90.7226032635016,174.458984880958,53.8680188065001));
#20427=CARTESIAN_POINT('Ctrl Pts',(-85.3800570143097,147.004359733543,57.1383954883763));
#20428=CARTESIAN_POINT('Ctrl Pts',(-52.4930107984057,166.104798004517,41.6778593074336));
#20429=CARTESIAN_POINT('Ctrl Pts',(-90.9233240871832,174.390787586828,53.4968768418598));
#20430=CARTESIAN_POINT('Ctrl Pts',(-85.7076058638931,146.813630884585,56.0739089930283));
#20431=CARTESIAN_POINT('Ctrl Pts',(-52.130067443758,166.415353901805,41.7330271353183));
#20432=CARTESIAN_POINT('Ctrl Pts',(-91.2985385599009,174.262722433064,52.7517362951234));
#20433=CARTESIAN_POINT('Ctrl Pts',(-85.8601535980719,146.72443849077,55.5388388898697));
#20434=CARTESIAN_POINT('Ctrl Pts',(-51.9524059049901,166.56629536905,41.7838517318022));
#20435=CARTESIAN_POINT('Ctrl Pts',(-91.473425281088,174.202723928459,52.3771872229046));
#20436=CARTESIAN_POINT('Ctrl Pts',(-86.2840014488134,146.475862855443,53.9250716815212));
#20437=CARTESIAN_POINT('Ctrl Pts',(-51.4370137885404,167.001978667705,42.0026128108074));
#20438=CARTESIAN_POINT('Ctrl Pts',(-91.9596328391763,174.03528173318,51.2475501770734));
#20439=CARTESIAN_POINT('Ctrl Pts',(-86.5215572476422,146.335470001124,52.8378286338531));
#20440=CARTESIAN_POINT('Ctrl Pts',(-51.1225180710597,167.264794255433,42.2370323177161));
#20441=CARTESIAN_POINT('Ctrl Pts',(-92.2325526199218,173.940389301699,50.4864800436924));
#20442=CARTESIAN_POINT('Ctrl Pts',(-86.9048658142535,146.108158385538,50.639890051958));
#20443=CARTESIAN_POINT('Ctrl Pts',(-50.5901985332046,167.707523804762,42.8482236974603));
#20444=CARTESIAN_POINT('Ctrl Pts',(-92.6732256277408,173.786512852862,48.9479230363755));
#20445=CARTESIAN_POINT('Ctrl Pts',(-87.050627720092,146.02123567785,49.5291966979117));
#20446=CARTESIAN_POINT('Ctrl Pts',(-50.3747927527441,167.885405901664,43.2250058043474));
#20447=CARTESIAN_POINT('Ctrl Pts',(-92.8409885630906,173.727526790654,48.1704376885321));
#20448=CARTESIAN_POINT('Ctrl Pts',(-87.2468358858299,145.904087274001,47.2833282524998));
#20449=CARTESIAN_POINT('Ctrl Pts',(-50.0788716488328,168.129413435683,44.066695404472));
#20450=CARTESIAN_POINT('Ctrl Pts',(-93.0668677799616,173.647986546177,46.598329776756));
#20451=CARTESIAN_POINT('Ctrl Pts',(-87.297297297057,145.873856069651,46.1481485313624));
#20452=CARTESIAN_POINT('Ctrl Pts',(-50.0000000004664,168.194190488835,44.5295600305827));
#20453=CARTESIAN_POINT('Ctrl Pts',(-93.1249999997334,173.62742978858,45.803703971949));
#20454=CARTESIAN_POINT('Ctrl Pts',(-87.2972972972973,145.873856069507,45.0000000000001));
#20455=CARTESIAN_POINT('Ctrl Pts',(-50.0000000000001,168.194190489106,45.));
#20456=CARTESIAN_POINT('Ctrl Pts',(-93.125,173.627429788614,45.0000000000001));
#20457=CARTESIAN_POINT('Ctrl Pts',(-87.2972972972973,145.873856069507,-45.));
#20458=CARTESIAN_POINT('Ctrl Pts',(-50.,168.194190489106,-45.));
#20459=CARTESIAN_POINT('Ctrl Pts',(-93.125,173.627429788614,-45.));
#20460=CARTESIAN_POINT('Ctrl Pts',(-87.2972972971987,145.873856069566,-46.1481557420891));
#20461=CARTESIAN_POINT('Ctrl Pts',(-50.0000000004424,168.194190488739,-44.5295601183673));
#20462=CARTESIAN_POINT('Ctrl Pts',(-93.1249999998352,173.627429788593,-45.8037090194605));
#20463=CARTESIAN_POINT('Ctrl Pts',(-87.2468342072022,145.90408834183,-47.2836204764629));
#20464=CARTESIAN_POINT('Ctrl Pts',(-50.07887561782,168.129410327578,-44.0665685622004));
#20465=CARTESIAN_POINT('Ctrl Pts',(-93.06686582199,173.647987290785,-46.5985343335265));
#20466=CARTESIAN_POINT('Ctrl Pts',(-87.0504855774481,146.021320480162,-49.5305505033));
#20467=CARTESIAN_POINT('Ctrl Pts',(-50.3750045511616,167.885231095311,-43.22451839411));
#20468=CARTESIAN_POINT('Ctrl Pts',(-92.8408249508251,173.727584349276,-48.1713853523075));
#20469=CARTESIAN_POINT('Ctrl Pts',(-86.9045853411086,146.108325679447,-50.6420203314529));
#20470=CARTESIAN_POINT('Ctrl Pts',(-50.5906119841123,167.70718247082,-42.8475063288785));
#20471=CARTESIAN_POINT('Ctrl Pts',(-92.6729028059307,173.7866263903,-48.9494142320252));
#20472=CARTESIAN_POINT('Ctrl Pts',(-86.5207468489932,146.335949618861,-52.8419520617065));
#20473=CARTESIAN_POINT('Ctrl Pts',(-51.1236121852308,167.263881768268,-42.236016926739));
#20474=CARTESIAN_POINT('Ctrl Pts',(-92.231621315453,173.940713684159,-50.4893664431864));
#20475=CARTESIAN_POINT('Ctrl Pts',(-86.2827997893804,146.476572189292,-53.930411905424));
#20476=CARTESIAN_POINT('Ctrl Pts',(-51.4385779165005,167.000669358337,-42.0015322603363));
#20477=CARTESIAN_POINT('Ctrl Pts',(-91.9582526161004,174.03576092614,-51.2512883338007));
#20478=CARTESIAN_POINT('Ctrl Pts',(-85.8580915626072,146.725645502692,-55.5463038168551));
#20479=CARTESIAN_POINT('Ctrl Pts',(-51.9548424687745,166.564229188848,-41.7830254980675));
#20480=CARTESIAN_POINT('Ctrl Pts',(-91.471060754875,174.203536282685,-52.3824126717966));
#20481=CARTESIAN_POINT('Ctrl Pts',(-85.7052114634742,146.815029246798,-56.0821321396214));
#20482=CARTESIAN_POINT('Ctrl Pts',(-52.1328160383236,166.413014140323,-41.7323431781605));
#20483=CARTESIAN_POINT('Ctrl Pts',(-91.295794141676,174.263662608782,-52.7574924977414));
#20484=CARTESIAN_POINT('Ctrl Pts',(-85.3768924607479,147.006198231513,-57.1482305947251));
#20485=CARTESIAN_POINT('Ctrl Pts',(-52.4964140404309,166.10187378431,-41.6776104852154));
#20486=CARTESIAN_POINT('Ctrl Pts',(-90.9197006272883,174.392020784196,-53.5037614163011));
#20487=CARTESIAN_POINT('Ctrl Pts',(-85.201572980522,147.107910335063,-57.6778553276653));
#20488=CARTESIAN_POINT('Ctrl Pts',(-52.6815987230577,165.942332214323,-41.6733918796236));
#20489=CARTESIAN_POINT('Ctrl Pts',(-90.7190119102538,174.460202437778,-53.8744987293807));
#20490=CARTESIAN_POINT('Ctrl Pts',(-84.6485098428038,147.427307739811,-59.2411239335854));
#20491=CARTESIAN_POINT('Ctrl Pts',(-53.2310695420675,165.46465987102,-41.730247968301));
#20492=CARTESIAN_POINT('Ctrl Pts',(-90.0864769882907,174.673866265291,-54.9687867534798));
#20493=CARTESIAN_POINT('Ctrl Pts',(-84.2419452441406,147.660259181751,-60.2551804226534));
#20494=CARTESIAN_POINT('Ctrl Pts',(-53.5952858098106,165.142447362445,-41.8585442148455));
#20495=CARTESIAN_POINT('Ctrl Pts',(-89.6221944884166,174.829143356289,-55.6786262958786));
#20496=CARTESIAN_POINT('Ctrl Pts',(-83.3589636976755,148.160523255651,-62.2322272830292));
#20497=CARTESIAN_POINT('Ctrl Pts',(-54.2798557221847,164.519102036724,-42.2830504688397));
#20498=CARTESIAN_POINT('Ctrl Pts',(-88.6159962195585,175.16089290001,-57.0625590980993));
#20499=CARTESIAN_POINT('Ctrl Pts',(-82.8825282275814,148.427846133224,-63.1952037501853));
#20500=CARTESIAN_POINT('Ctrl Pts',(-54.6002746634411,164.218288168885,-42.5752870988414));
#20501=CARTESIAN_POINT('Ctrl Pts',(-88.0740596024118,175.33737196623,-57.7366426251549));
#20502=CARTESIAN_POINT('Ctrl Pts',(-81.8638978961899,148.992084401777,-65.0739651883141));
#20503=CARTESIAN_POINT('Ctrl Pts',(-55.1703038853821,163.656479580582,-43.3013319230022));
#20504=CARTESIAN_POINT('Ctrl Pts',(-86.9181045359956,175.70764400461,-59.0517756317946));
#20505=CARTESIAN_POINT('Ctrl Pts',(-81.3216912305501,149.289006692322,-65.9897411795777));
#20506=CARTESIAN_POINT('Ctrl Pts',(-55.4209153337387,163.395146817933,-43.7313440943059));
#20507=CARTESIAN_POINT('Ctrl Pts',(-86.3040727099585,175.90144153157,-59.6928188257368));
#20508=CARTESIAN_POINT('Ctrl Pts',(-80.4611806720501,149.75347959498,-67.3302212152897));
#20509=CARTESIAN_POINT('Ctrl Pts',(-55.7323628889726,163.039374353445,-44.4659089553466));
#20510=CARTESIAN_POINT('Ctrl Pts',(-85.3320488395596,176.202519245937,-60.6311548506866));
#20511=CARTESIAN_POINT('Ctrl Pts',(-80.1660792196943,149.911692897809,-67.7720166440731));
#20512=CARTESIAN_POINT('Ctrl Pts',(-55.8249508600411,162.927551611724,-44.7233355746148));
#20513=CARTESIAN_POINT('Ctrl Pts',(-84.9990979101181,176.304741064775,-60.9404116508692));
#20514=CARTESIAN_POINT('Ctrl Pts',(-79.5649495321451,150.231603635495,-68.638474298271));
#20515=CARTESIAN_POINT('Ctrl Pts',(-55.9858061786668,162.71878843487,-45.2587322589989));
#20516=CARTESIAN_POINT('Ctrl Pts',(-84.3217302379204,176.510695829274,-61.5469320087717));
#20517=CARTESIAN_POINT('Ctrl Pts',(-79.2584561448351,150.393554949854,-69.0639054241725));
#20518=CARTESIAN_POINT('Ctrl Pts',(-56.0545272978165,162.621495302187,-45.5367648107279));
#20519=CARTESIAN_POINT('Ctrl Pts',(-83.9767870352385,176.614594219734,-61.8447337969382));
#20520=CARTESIAN_POINT('Ctrl Pts',(-77.6976281010343,151.211991727362,-71.1542377786429));
#20521=CARTESIAN_POINT('Ctrl Pts',(-56.3329566915923,162.17877220309,-46.946790015033));
#20522=CARTESIAN_POINT('Ctrl Pts',(-82.2224229503939,177.137674896828,-63.3079664449803));
#20523=CARTESIAN_POINT('Ctrl Pts',(-76.358755256544,151.894158252871,-72.7094834320272));
#20524=CARTESIAN_POINT('Ctrl Pts',(-56.3753525382564,161.929333704007,-48.2248892798433));
#20525=CARTESIAN_POINT('Ctrl Pts',(-80.7247115749601,177.567361482489,-64.3966384024778));
#20526=CARTESIAN_POINT('Ctrl Pts',(-73.5232682991988,153.286737307182,-75.6262347306282));
#20527=CARTESIAN_POINT('Ctrl Pts',(-56.0769147808614,161.64396004567,-50.8934787988654));
#20528=CARTESIAN_POINT('Ctrl Pts',(-77.5709436079268,178.428009730871,-66.438364311381));
#20529=CARTESIAN_POINT('Ctrl Pts',(-72.026462046429,153.997283676109,-76.9874494541838));
#20530=CARTESIAN_POINT('Ctrl Pts',(-55.7533758428049,161.598527556718,-52.277798604289));
#20531=CARTESIAN_POINT('Ctrl Pts',(-75.9146586641507,178.859068766111,-67.3912146179833));
#20532=CARTESIAN_POINT('Ctrl Pts',(-69.6720528505947,155.069496372499,-78.9024214954926));
#20533=CARTESIAN_POINT('Ctrl Pts',(-55.0037430741423,161.657376274586,-54.3817685485241));
#20534=CARTESIAN_POINT('Ctrl Pts',(-73.3245273944502,179.494497920776,-68.7316950468175));
#20535=CARTESIAN_POINT('Ctrl Pts',(-68.8668727613371,155.42891241544,-79.5209801538095));
#20536=CARTESIAN_POINT('Ctrl Pts',(-54.7157160376554,161.696600504129,-55.0782117530934));
#20537=CARTESIAN_POINT('Ctrl Pts',(-72.4411497039392,179.704994726958,-69.1646861076988));
#20538=CARTESIAN_POINT('Ctrl Pts',(-67.2348038674229,156.14183977231,-80.708101155254));
#20539=CARTESIAN_POINT('Ctrl Pts',(-54.066973497348,161.809518307269,-56.4530352471832));
#20540=CARTESIAN_POINT('Ctrl Pts',(-70.6556461223016,180.117114694266,-69.9956708086456));
#20541=CARTESIAN_POINT('Ctrl Pts',(-66.4074631994888,156.495603406397,-81.2772464428291));
#20542=CARTESIAN_POINT('Ctrl Pts',(-53.7077907544062,161.88241013336,-57.1322849215662));
#20543=CARTESIAN_POINT('Ctrl Pts',(-69.7530076022098,180.31890347519,-70.3940725100073));
#20544=CARTESIAN_POINT('Ctrl Pts',(-63.8933382808409,157.546632905389,-82.9176021366126));
#20545=CARTESIAN_POINT('Ctrl Pts',(-52.5438986519127,162.140391064739,-59.1171215542775));
#20546=CARTESIAN_POINT('Ctrl Pts',(-67.0176814730437,180.909823248112,-71.5423214955749));
#20547=CARTESIAN_POINT('Ctrl Pts',(-62.174543902428,158.233573752389,-83.9220069329356));
#20548=CARTESIAN_POINT('Ctrl Pts',(-51.6366986179836,162.366801122918,-60.4123360466614));
#20549=CARTESIAN_POINT('Ctrl Pts',(-65.157696820993,181.284462131077,-72.2454048531114));
#20550=CARTESIAN_POINT('Ctrl Pts',(-58.6583288600459,159.570480438189,-85.7767676195814));
#20551=CARTESIAN_POINT('Ctrl Pts',(-49.6036015941499,162.891141744692,-62.889235475676));
#20552=CARTESIAN_POINT('Ctrl Pts',(-61.3733230166759,181.987898288311,-73.5437373336506));
#20553=CARTESIAN_POINT('Ctrl Pts',(-56.8608714195449,160.220477504758,-86.6270094856871));
#20554=CARTESIAN_POINT('Ctrl Pts',(-48.4845845503338,163.186764146197,-64.0761818103832));
#20555=CARTESIAN_POINT('Ctrl Pts',(-59.4488880520778,182.316719637853,-74.1389066400079));
#20556=CARTESIAN_POINT('Ctrl Pts',(-53.1914516507995,161.475786363539,-88.1898645846761));
#20557=CARTESIAN_POINT('Ctrl Pts',(-46.061615193226,163.817511046626,-66.3291607861143));
#20558=CARTESIAN_POINT('Ctrl Pts',(-55.5408149349383,182.922547542729,-75.2329052092463));
#20559=CARTESIAN_POINT('Ctrl Pts',(-51.319470175582,162.081117268138,-88.902415984378));
#20560=CARTESIAN_POINT('Ctrl Pts',(-44.7628166978043,164.151587900672,-67.4001257057399));
#20561=CARTESIAN_POINT('Ctrl Pts',(-53.5571522154415,183.199569273526,-75.7316911890953));
#20562=CARTESIAN_POINT('Ctrl Pts',(-48.4573974379579,162.950528633808,-89.8766149078073));
#20563=CARTESIAN_POINT('Ctrl Pts',(-42.6777574357427,164.667756974113,-68.9266888034224));
#20564=CARTESIAN_POINT('Ctrl Pts',(-50.5395813143088,183.572219031567,-76.4136304354497));
#20565=CARTESIAN_POINT('Ctrl Pts',(-47.4925380968551,163.234409214934,-90.1860654079167));
#20566=CARTESIAN_POINT('Ctrl Pts',(-41.9675064328372,164.840576291436,-69.4179616869902));
#20567=CARTESIAN_POINT('Ctrl Pts',(-49.5248053055096,183.689484703437,-76.6302457855649));
#20568=CARTESIAN_POINT('Ctrl Pts',(-45.5559253860908,163.785442542513,-90.7712192710136));
#20569=CARTESIAN_POINT('Ctrl Pts',(-40.517921424902,165.185340070797,-70.3652778060076));
#20570=CARTESIAN_POINT('Ctrl Pts',(-47.4929604819986,183.907885928098,-77.0398534896864));
#20571=CARTESIAN_POINT('Ctrl Pts',(-44.5840993906858,164.052662821325,-91.0470382563051));
#20572=CARTESIAN_POINT('Ctrl Pts',(-39.7788834259429,165.357345411408,-70.8220737068328));
#20573=CARTESIAN_POINT('Ctrl Pts',(-46.4758027387637,184.009072193089,-77.2329267794284));
#20574=CARTESIAN_POINT('Ctrl Pts',(-41.6583648757858,164.829163150394,-91.8271696738661));
#20575=CARTESIAN_POINT('Ctrl Pts',(-37.5386431096872,165.865096098891,-72.1323233720483));
#20576=CARTESIAN_POINT('Ctrl Pts',(-43.4207826222858,184.288457643329,-77.7790187716767));
#20577=CARTESIAN_POINT('Ctrl Pts',(-39.6942137926577,165.31328171977,-92.2842750101778));
#20578=CARTESIAN_POINT('Ctrl Pts',(-35.9826718196518,166.200468258917,-72.9482919924133));
#20579=CARTESIAN_POINT('Ctrl Pts',(-41.3793866364986,184.44248647661,-78.0989925071645));
#20580=CARTESIAN_POINT('Ctrl Pts',(-33.7626089079634,166.662932669615,-93.4851484356314));
#20581=CARTESIAN_POINT('Ctrl Pts',(-31.2448533153792,167.153811440344,-75.175023213843));
#20582=CARTESIAN_POINT('Ctrl Pts',(-35.2417468235887,184.806791744904,-78.9396039048619));
#20583=CARTESIAN_POINT('Ctrl Pts',(-29.7561551119682,167.425823856563,-94.0596464150218));
#20584=CARTESIAN_POINT('Ctrl Pts',(-27.8711969032041,167.75000000849,-76.447793000883));
#20585=CARTESIAN_POINT('Ctrl Pts',(-31.1321796448434,184.919391068587,-79.341752490545));
#20586=CARTESIAN_POINT('Ctrl Pts',(-21.6443130141392,168.666413299276,-94.8172777838099));
#20587=CARTESIAN_POINT('Ctrl Pts',(-20.8545946334258,168.752931245308,-78.5305497139422));
#20588=CARTESIAN_POINT('Ctrl Pts',(-22.8769266922517,184.876461117654,-79.8720944486372));
#20589=CARTESIAN_POINT('Ctrl Pts',(-17.5388295044679,169.144191789785,-95.));
#20590=CARTESIAN_POINT('Ctrl Pts',(-17.2137406264089,169.169866026837,-79.3645543485074));
#20591=CARTESIAN_POINT('Ctrl Pts',(-18.7311428158619,184.720985760753,-80.));
#20592=CARTESIAN_POINT('Ctrl Pts',(-13.3842538190364,169.472303783561,-95.));
#20593=CARTESIAN_POINT('Ctrl Pts',(-13.3842538190364,169.472303783561,-80.));
#20594=CARTESIAN_POINT('Ctrl Pts',(-14.5652173913043,184.425742352699,-80.));
#20595=CARTESIAN_POINT('Origin',(-14.5652173913044,184.425742352699,-95.));
#20596=CARTESIAN_POINT('Origin',(0.,0.,-95.));
#20597=CARTESIAN_POINT('Origin',(65.4347826086956,173.041293409847,-95.));
#20598=CARTESIAN_POINT('Ctrl Pts',(60.1111342549551,159.017771142991,-94.9999991819279));
#20599=CARTESIAN_POINT('Ctrl Pts',(60.112229341533,159.017357178332,-79.9970998734751));
#20600=CARTESIAN_POINT('Ctrl Pts',(65.417178607917,173.051048440272,-79.9999995062288));
#20601=CARTESIAN_POINT('Ctrl Pts',(64.2759087790417,157.443422060874,-95.0003751304781));
#20602=CARTESIAN_POINT('Ctrl Pts',(63.9530157134296,157.565450775654,-80.5517566472176));
#20603=CARTESIAN_POINT('Ctrl Pts',(69.4980685405773,170.904779447422,-80.0002460391242));
#20604=CARTESIAN_POINT('Ctrl Pts',(68.3475790492405,155.717622096499,-94.871163811165));
#20605=CARTESIAN_POINT('Ctrl Pts',(67.839523093928,155.937210710705,-80.9562034651419));
#20606=CARTESIAN_POINT('Ctrl Pts',(73.4707419831936,168.632424521765,-79.9097827170611));
#20607=CARTESIAN_POINT('Ctrl Pts',(76.3074783717944,151.975267654439,-94.3981030531305));
#20608=CARTESIAN_POINT('Ctrl Pts',(75.4920654425922,152.377267494459,-81.4803630768627));
#20609=CARTESIAN_POINT('Ctrl Pts',(81.2094587552533,163.843390510905,-79.5786121633006));
#20610=CARTESIAN_POINT('Ctrl Pts',(80.1959679692073,149.959099180745,-94.0543379212976));
#20611=CARTESIAN_POINT('Ctrl Pts',(79.2729405895899,150.450643093642,-81.610159134502));
#20612=CARTESIAN_POINT('Ctrl Pts',(84.9757898620679,161.327031076194,-79.3379638009463));
#20613=CARTESIAN_POINT('Ctrl Pts',(87.8000684551132,145.637470058004,-93.1809712878189));
#20614=CARTESIAN_POINT('Ctrl Pts',(86.7038679660169,146.292589564658,-81.6312588884628));
#20615=CARTESIAN_POINT('Ctrl Pts',(92.3178905891635,156.046341746203,-78.7265842415997));
#20616=CARTESIAN_POINT('Ctrl Pts',(91.5156662167745,143.332003833586,-92.6512484049633));
#20617=CARTESIAN_POINT('Ctrl Pts',(90.3665685559524,144.064645405084,-81.5291708234098));
#20618=CARTESIAN_POINT('Ctrl Pts',(95.8936350663941,153.282013745197,-78.3557679793618));
#20619=CARTESIAN_POINT('Ctrl Pts',(96.9597420465583,139.655302598139,-91.7313856490923));
#20620=CARTESIAN_POINT('Ctrl Pts',(95.7862627909755,140.469122838069,-81.2184414032456));
#20621=CARTESIAN_POINT('Ctrl Pts',(101.118204141379,148.945321268586,-77.7118507119895));
#20622=CARTESIAN_POINT('Ctrl Pts',(98.7528522876294,138.393276733977,-91.4038190221124));
#20623=CARTESIAN_POINT('Ctrl Pts',(97.5656444562283,139.240074531893,-81.090445379421));
#20624=CARTESIAN_POINT('Ctrl Pts',(102.83651907572,147.468018852879,-77.482549883046));
#20625=CARTESIAN_POINT('Ctrl Pts',(102.295631429099,135.795539951176,-90.7084745843493));
#20626=CARTESIAN_POINT('Ctrl Pts',(101.08836342036,136.704210068963,-80.7859436045695));
#20627=CARTESIAN_POINT('Ctrl Pts',(106.226989111109,144.448761779836,-76.9958010076012));
#20628=CARTESIAN_POINT('Ctrl Pts',(104.036759724654,134.466015015237,-90.3423416599025));
#20629=CARTESIAN_POINT('Ctrl Pts',(102.824700624036,135.403548229412,-80.6106071343671));
#20630=CARTESIAN_POINT('Ctrl Pts',(107.890968825064,142.914010738197,-76.7395043944721));
#20631=CARTESIAN_POINT('Ctrl Pts',(109.159801879624,130.396180641668,-89.1948681948962));
#20632=CARTESIAN_POINT('Ctrl Pts',(107.914041417891,131.435704885724,-80.0241711884031));
#20633=CARTESIAN_POINT('Ctrl Pts',(112.780952607655,138.245372543666,-75.9362630669522));
#20634=CARTESIAN_POINT('Ctrl Pts',(112.446820922312,127.570888947651,-88.3636043219537));
#20635=CARTESIAN_POINT('Ctrl Pts',(111.217729898413,128.654798668491,-79.5479026354358));
#20636=CARTESIAN_POINT('Ctrl Pts',(115.910241206126,135.042722405181,-75.3543730932938));
#20637=CARTESIAN_POINT('Ctrl Pts',(118.773955285056,121.701958851828,-86.5841254176429));
#20638=CARTESIAN_POINT('Ctrl Pts',(117.585782049815,122.85919246317,-78.4483848675869));
#20639=CARTESIAN_POINT('Ctrl Pts',(121.921081617715,128.457279136201,-74.1087296370299));
#20640=CARTESIAN_POINT('Ctrl Pts',(121.814041889342,118.658306100528,-85.6358543716128));
#20641=CARTESIAN_POINT('Ctrl Pts',(120.66102035423,119.843166235463,-77.8267940587746));
#20642=CARTESIAN_POINT('Ctrl Pts',(124.802595789209,125.074482642951,-73.4449369322121));
#20643=CARTESIAN_POINT('Ctrl Pts',(127.651676978735,112.354366949315,-83.6326763250667));
#20644=CARTESIAN_POINT('Ctrl Pts',(126.571701813616,113.579870675594,-76.4540968745708));
#20645=CARTESIAN_POINT('Ctrl Pts',(130.325562248462,118.125822143933,-72.0427084706124));
#20646=CARTESIAN_POINT('Ctrl Pts',(130.449215516193,109.094078884125,-82.5777372262417));
#20647=CARTESIAN_POINT('Ctrl Pts',(129.416365557056,110.330915238904,-75.7039088453632));
#20648=CARTESIAN_POINT('Ctrl Pts',(132.966997945925,114.559964695876,-71.3042502449321));
#20649=CARTESIAN_POINT('Ctrl Pts',(133.794311682363,104.882026123237,-81.1964639412298));
#20650=CARTESIAN_POINT('Ctrl Pts',(132.838493559395,106.10134488633,-74.6872762872343));
#20651=CARTESIAN_POINT('Ctrl Pts',(136.120374355175,109.984367092914,-70.3373593035059));
#20652=CARTESIAN_POINT('Ctrl Pts',(134.455728161623,104.032771605557,-80.9170710194717));
#20653=CARTESIAN_POINT('Ctrl Pts',(133.511839282076,105.252753778121,-74.4814177849335));
#20654=CARTESIAN_POINT('Ctrl Pts',(136.743616908387,109.063325218641,-70.1417843510365));
#20655=CARTESIAN_POINT('Ctrl Pts',(135.763304172496,102.320504511913,-80.3520788936114));
#20656=CARTESIAN_POINT('Ctrl Pts',(134.843563817047,103.540882681733,-74.0625229865155));
#20657=CARTESIAN_POINT('Ctrl Pts',(137.975229665001,107.209266271442,-69.7462901692913));
#20658=CARTESIAN_POINT('Ctrl Pts',(136.409901038833,101.456869632053,-80.0662719859412));
#20659=CARTESIAN_POINT('Ctrl Pts',(135.502515214701,102.676936647862,-73.8493312768616));
#20660=CARTESIAN_POINT('Ctrl Pts',(138.58401109663,106.275579593581,-69.54622554808));
#20661=CARTESIAN_POINT('Ctrl Pts',(138.319688906544,98.8549121118194,-79.2028595772069));
#20662=CARTESIAN_POINT('Ctrl Pts',(137.446226650836,100.077150239795,-73.2027294103901));
#20663=CARTESIAN_POINT('Ctrl Pts',(140.38141096588,103.466810344861,-68.9418376391995));
#20664=CARTESIAN_POINT('Ctrl Pts',(139.554945257284,97.1029464010168,-78.6184167040672));
#20665=CARTESIAN_POINT('Ctrl Pts',(138.707397076576,98.3214899139818,-72.7594319021101));
#20666=CARTESIAN_POINT('Ctrl Pts',(141.543035412226,101.581203667191,-68.5327284081521));
#20667=CARTESIAN_POINT('Ctrl Pts',(145.545768022881,88.257965867027,-75.6545459910273));
#20668=CARTESIAN_POINT('Ctrl Pts',(144.769209545676,89.5336250768842,-70.5112314979136));
#20669=CARTESIAN_POINT('Ctrl Pts',(147.172811037201,92.0873797452005,-66.4580231276975));
#20670=CARTESIAN_POINT('Ctrl Pts',(149.748394839051,80.9109007292597,-73.1515201298415));
#20671=CARTESIAN_POINT('Ctrl Pts',(149.10565652523,82.1186746566399,-68.5241447747446));
#20672=CARTESIAN_POINT('Ctrl Pts',(151.109449611751,84.2828338177688,-64.7059126364692));
#20673=CARTESIAN_POINT('Ctrl Pts',(155.204094851673,69.494444703847,-69.2286486640292));
#20674=CARTESIAN_POINT('Ctrl Pts',(154.735913995021,70.5418248776468,-65.3361268068727));
#20675=CARTESIAN_POINT('Ctrl Pts',(156.211187623449,72.2434629686532,-61.9599183141271));
#20676=CARTESIAN_POINT('Ctrl Pts',(156.880610977566,65.6227064855729,-67.8926978273502));
#20677=CARTESIAN_POINT('Ctrl Pts',(156.462811525529,66.6261512215435,-64.244358760138));
#20678=CARTESIAN_POINT('Ctrl Pts',(157.777199743145,68.1747130437632,-61.0247584927152));
#20679=CARTESIAN_POINT('Ctrl Pts',(159.181124815175,59.7146207337219,-65.8479415996448));
#20680=CARTESIAN_POINT('Ctrl Pts',(158.835393856705,60.6370847202265,-62.5584808650695));
#20681=CARTESIAN_POINT('Ctrl Pts',(159.924440842033,61.9838631282589,-59.5934387405923));
#20682=CARTESIAN_POINT('Ctrl Pts',(159.912213965834,57.7284955928914,-65.1595391421529));
#20683=CARTESIAN_POINT('Ctrl Pts',(159.588605204181,58.6261359764456,-61.9898219706128));
#20684=CARTESIAN_POINT('Ctrl Pts',(160.606519600763,59.9056104900601,-59.1115603374229));
#20685=CARTESIAN_POINT('Ctrl Pts',(160.954720457779,54.7238687144498,-64.1168149426715));
#20686=CARTESIAN_POINT('Ctrl Pts',(160.663581109104,55.5804420657701,-61.1251183797621));
#20687=CARTESIAN_POINT('Ctrl Pts',(161.578790543905,56.765595205057,-58.381658600695));
#20688=CARTESIAN_POINT('Ctrl Pts',(161.29348368791,53.7171877676969,-63.7672407290392));
#20689=CARTESIAN_POINT('Ctrl Pts',(161.012707512599,54.5605741899303,-60.8350012513618));
#20690=CARTESIAN_POINT('Ctrl Pts',(161.894669312994,55.7142130829498,-58.1369584136762));
#20691=CARTESIAN_POINT('Ctrl Pts',(161.950956676582,51.7011776789652,-63.0667763221531));
#20692=CARTESIAN_POINT('Ctrl Pts',(161.690355251076,52.5177903828148,-60.2528453749454));
#20693=CARTESIAN_POINT('Ctrl Pts',(162.507622025497,53.6099267097544,-57.6466369090903));
#20694=CARTESIAN_POINT('Ctrl Pts',(162.269760743618,50.6916407801757,-62.7158144756995));
#20695=CARTESIAN_POINT('Ctrl Pts',(162.019036838256,51.4945755273328,-59.9607244911299));
#20696=CARTESIAN_POINT('Ctrl Pts',(162.804784047433,52.5568039581638,-57.4009654354441));
#20697=CARTESIAN_POINT('Ctrl Pts',(165.050384665975,41.5921040025995,-59.5507777161095));
#20698=CARTESIAN_POINT('Ctrl Pts',(164.871359484215,42.3174710736492,-57.3363962733902));
#20699=CARTESIAN_POINT('Ctrl Pts',(165.396228187219,43.0696062134821,-55.1854558426586));
#20700=CARTESIAN_POINT('Ctrl Pts',(166.895487919146,33.4066584132222,-56.6925205986574));
#20701=CARTESIAN_POINT('Ctrl Pts',(166.788260729585,33.9828141264701,-54.9228164063036));
#20702=CARTESIAN_POINT('Ctrl Pts',(167.112953987927,34.5721559092001,-53.184692547786));
#20703=CARTESIAN_POINT('Ctrl Pts',(168.751767516731,20.9849502860056,-52.3482901797354));
#20704=CARTESIAN_POINT('Ctrl Pts',(168.708840626242,21.3425904821289,-51.2420487454299));
#20705=CARTESIAN_POINT('Ctrl Pts',(168.839541543698,21.7037023388406,-50.1437575153319));
#20706=CARTESIAN_POINT('Ctrl Pts',(169.217967102393,16.8203670205984,-50.8906501981523));
#20707=CARTESIAN_POINT('Ctrl Pts',(169.191375205316,17.1062528224251,-50.0050582315602));
#20708=CARTESIAN_POINT('Ctrl Pts',(169.272994225589,17.3937906443598,-49.1234184860096));
#20709=CARTESIAN_POINT('Ctrl Pts',(169.686138855138,10.5368669289468,-48.6905305277644));
#20710=CARTESIAN_POINT('Ctrl Pts',(169.675477965606,10.7154189671323,-48.1364420820892));
#20711=CARTESIAN_POINT('Ctrl Pts',(169.70824473707,10.8943962209014,-47.5833483506363));
#20712=CARTESIAN_POINT('Ctrl Pts',(169.803634766947,8.43625666946546,-47.9548772374033));
#20713=CARTESIAN_POINT('Ctrl Pts',(169.796983992598,8.57911136209104,-47.5113888418552));
#20714=CARTESIAN_POINT('Ctrl Pts',(169.817467420272,8.72217091739304,-47.0683956245868));
#20715=CARTESIAN_POINT('Ctrl Pts',(169.96062524395,4.22263819730324,-46.4790883105662));
#20716=CARTESIAN_POINT('Ctrl Pts',(169.959277927784,4.29443906381557,-46.2573336232601));
#20717=CARTESIAN_POINT('Ctrl Pts',(169.96340072668,4.36546597331119,-46.0353525730877));
#20718=CARTESIAN_POINT('Ctrl Pts',(170.,2.10804680144307,-45.7383979468224));
#20719=CARTESIAN_POINT('Ctrl Pts',(170.,2.1436981469272,-45.6276358930879));
#20720=CARTESIAN_POINT('Ctrl Pts',(170.,2.17934967138514,-45.516873902782));
#20721=CARTESIAN_POINT('Ctrl Pts',(170.,0.,-45.));
#20722=CARTESIAN_POINT('Ctrl Pts',(170.,0.,-45.));
#20723=CARTESIAN_POINT('Ctrl Pts',(170.,0.,-45.));
#20724=CARTESIAN_POINT('Origin',(0.,0.,-95.));
#20725=CARTESIAN_POINT('Origin',(0.,0.,-95.));
#20726=CARTESIAN_POINT('Origin',(-115.,0.,-105.));
#20727=CARTESIAN_POINT('',(-95.6492560750855,183.985186114405,-44.9999999999999));
#20728=CARTESIAN_POINT('Origin',(-115.,0.,-44.9999999999999));
#20729=CARTESIAN_POINT('',(-95.6492560750855,183.985186114405,45.0000000000001));
#20730=CARTESIAN_POINT('',(-95.6492560750855,183.985186114405,-105.));
#20731=CARTESIAN_POINT('Origin',(-115.,0.,45.0000000000001));
#20732=CARTESIAN_POINT('Origin',(-115.000000000001,175.,70.0000000000001));
#20733=CARTESIAN_POINT('',(-93.0342906798268,208.848049102839,70.0000000000001));
#20734=CARTESIAN_POINT('',(-14.5652173913043,184.425742352699,70.));
#20735=CARTESIAN_POINT('Origin',(-115.,0.,70.0000000000001));
#20736=CARTESIAN_POINT('',(-108.033967922038,209.585728186396,70.));
#20737=CARTESIAN_POINT('Origin',(-107.155103814224,74.5885889652995,70.0000000000001));
#20738=CARTESIAN_POINT('',(-108.033967922038,249.902929948988,70.0000000000001));
#20739=CARTESIAN_POINT('',(-108.033967922038,175.,70.0000000000001));
#20740=CARTESIAN_POINT('',(65.4347826086958,173.041293409847,70.));
#20741=CARTESIAN_POINT('Origin',(-115.,0.,70.0000000000001));
#20742=CARTESIAN_POINT('Origin',(-6.30808536718839E-15,0.,70.));
#20743=CARTESIAN_POINT('Origin',(-115.,0.,-105.));
#20744=CARTESIAN_POINT('',(-107.337364714242,274.893222943887,45.0000000000001));
#20745=CARTESIAN_POINT('Origin',(-115.,0.,45.0000000000001));
#20746=CARTESIAN_POINT('',(-115.000000000001,275.,45.1798442476467));
#20747=CARTESIAN_POINT('Origin',(-109.334804813311,203.273336013208,165.779888116268));
#20748=CARTESIAN_POINT('',(-115.000000000001,275.,-45.1798442476466));
#20749=CARTESIAN_POINT('',(-115.000000000001,275.,2.35800814060629E-28));
#20750=CARTESIAN_POINT('',(-107.337364714242,274.893222943887,-44.9999999999999));
#20751=CARTESIAN_POINT('Origin',(-109.334804813308,203.273336012913,-165.779888116317));
#20752=CARTESIAN_POINT('Origin',(-115.,0.,-44.9999999999999));
#20753=CARTESIAN_POINT('Origin',(-115.000000000001,175.,-70.));
#20754=CARTESIAN_POINT('',(-108.033967922038,249.902929948988,-69.9999999999999));
#20755=CARTESIAN_POINT('',(65.4347826086956,173.041293409847,-70.));
#20756=CARTESIAN_POINT('Origin',(-115.,0.,-70.));
#20757=CARTESIAN_POINT('',(-108.033967922038,209.585728186396,-70.));
#20758=CARTESIAN_POINT('',(-108.033967922038,175.,-70.));
#20759=CARTESIAN_POINT('',(-93.0342906798268,208.848049102839,-70.));
#20760=CARTESIAN_POINT('Origin',(-107.155103814224,74.5885889652995,-70.));
#20761=CARTESIAN_POINT('',(-14.5652173913044,184.425742352699,-70.));
#20762=CARTESIAN_POINT('Origin',(-115.,0.,-70.));
#20763=CARTESIAN_POINT('Origin',(6.30808536718839E-15,0.,-70.));
#20764=CARTESIAN_POINT('Origin',(-9.76996261670139E-13,275.,2.35800814060629E-28));
#20765=CARTESIAN_POINT('',(-126.751426934183,275.,46.3038641989654));
#20766=CARTESIAN_POINT('Origin',(-108.033967922038,275.,180.));
#20767=CARTESIAN_POINT('',(3.92135447228736,275.,28.0096748020595));
#20768=CARTESIAN_POINT('',(-126.751426934183,275.,-46.3038641989653));
#20769=CARTESIAN_POINT('',(3.92135447228734,275.,-28.0096748020595));
#20770=CARTESIAN_POINT('Origin',(-108.033967922039,275.,-180.));
#20771=CARTESIAN_POINT('Origin',(7.3875505856485,2.56307148617813E-14,52.7682184689178));
#20772=CARTESIAN_POINT('',(-130.164585944519,206.966980183574,72.0255175831412));
#20773=CARTESIAN_POINT('',(-36.8701707223189,225.625863228014,58.9642994520331));
#20774=CARTESIAN_POINT('',(-123.285230820823,250.,71.0624078658237));
#20775=CARTESIAN_POINT('',(7.38755058564849,250.,52.7682184689177));
#20776=CARTESIAN_POINT('',(-123.285230820823,208.15873578029,71.0624078658237));
#20777=CARTESIAN_POINT('',(-123.285230820823,2.56307148617813E-14,71.0624078658238));
#20778=CARTESIAN_POINT('Origin',(-103.70046162358,72.0502949994303,68.3205401782068));
#20779=CARTESIAN_POINT('Origin',(7.38755058564847,2.56307148617812E-14,
-52.7682184689177));
#20780=CARTESIAN_POINT('',(-123.285230820823,250.,-71.0624078658236));
#20781=CARTESIAN_POINT('',(-123.285230820823,208.15873578029,-71.0624078658236));
#20782=CARTESIAN_POINT('',(-123.285230820823,2.56307148617812E-14,-71.0624078658237));
#20783=CARTESIAN_POINT('',(7.38755058564846,249.999999999999,-52.7682184689176));
#20784=CARTESIAN_POINT('',(-130.164585944519,206.966980183574,-72.0255175831411));
#20785=CARTESIAN_POINT('',(-36.870170722319,225.625863228014,-58.964299452033));
#20786=CARTESIAN_POINT('Origin',(-103.700461599128,72.0502948555587,-68.3205401747857));
#20787=CARTESIAN_POINT('Origin',(-40.0380844283057,200.190422141525,9.66330504221541E-15));
#20788=CARTESIAN_POINT('',(-128.727878679424,182.452463291301,47.2669739162829));
#20789=CARTESIAN_POINT('',(-35.4334634572244,201.111346335741,34.2057557851749));
#20790=CARTESIAN_POINT('',(-128.727878679425,182.452463291301,-47.2669739162828));
#20791=CARTESIAN_POINT('',(-128.727878679425,182.452463291301,9.66330504221541E-15));
#20792=CARTESIAN_POINT('',(-35.4334634572244,201.111346335741,-34.2057557851748));
#20793=CARTESIAN_POINT('Origin',(-108.033967922037,-3.74818120714568E-13,
180.));
#20794=CARTESIAN_POINT('',(-113.709994059638,250.,70.1465397573418));
#20795=CARTESIAN_POINT('Origin',(-108.033967922038,250.,180.));
#20796=CARTESIAN_POINT('Origin',(-109.765188581363,199.310273833714,146.488884695692));
#20797=CARTESIAN_POINT('Ctrl Pts',(-123.285230820823,208.15873578029,71.0624078658237));
#20798=CARTESIAN_POINT('Ctrl Pts',(-120.772211061873,208.611218684362,70.7105850995707));
#20799=CARTESIAN_POINT('Ctrl Pts',(-118.243257051618,208.957585927806,70.4450832185436));
#20800=CARTESIAN_POINT('Ctrl Pts',(-115.698109518352,209.19624749802,70.267320575903));
#20801=CARTESIAN_POINT('Ctrl Pts',(-113.490059874391,209.40329899042,70.1131021132552));
#20802=CARTESIAN_POINT('Ctrl Pts',(-111.269812456632,209.529293532016,70.0249139423489));
#20803=CARTESIAN_POINT('Ctrl Pts',(-109.037063883093,209.572105119168,70.0045693065261));
#20804=CARTESIAN_POINT('Ctrl Pts',(-108.702978801238,209.578510996107,70.0015251485744));
#20805=CARTESIAN_POINT('Ctrl Pts',(-108.368613822657,209.583054418182,70.));
#20806=CARTESIAN_POINT('Ctrl Pts',(-108.033967922038,209.585728186396,70.));
#20807=CARTESIAN_POINT('Origin',(-107.155103814224,74.5885889652995,-105.));
#20808=CARTESIAN_POINT('',(-123.122478208265,183.423523407144,-46.3038641989653));
#20809=CARTESIAN_POINT('',(-107.87121530948,184.586257960267,-44.9999999999999));
#20810=CARTESIAN_POINT('Ctrl Pts',(-123.122478208265,183.423523407144,-46.3038641989653));
#20811=CARTESIAN_POINT('Ctrl Pts',(-120.609173163533,183.792255035655,-45.8720326960086));
#20812=CARTESIAN_POINT('Ctrl Pts',(-118.08021495677,184.07446046044,-45.5462136818661));
#20813=CARTESIAN_POINT('Ctrl Pts',(-115.535356905798,184.268903325358,-45.3280752522695));
#20814=CARTESIAN_POINT('Ctrl Pts',(-113.288417354346,184.440583377813,-45.1354736001008));
#20815=CARTESIAN_POINT('Ctrl Pts',(-111.029072640325,184.543852620633,-45.0268083769033));
#20816=CARTESIAN_POINT('Ctrl Pts',(-108.75701249268,184.576927773769,-45.004372785009));
#20817=CARTESIAN_POINT('Ctrl Pts',(-108.461961429881,184.581222932546,-45.0014592858925));
#20818=CARTESIAN_POINT('Ctrl Pts',(-108.166695930546,184.584334309781,-45.));
#20819=CARTESIAN_POINT('Ctrl Pts',(-107.87121530948,184.586257960267,-45.));
#20820=CARTESIAN_POINT('Origin',(-107.170701202847,71.4826465588299,-43.5630588770692));
#20821=CARTESIAN_POINT('',(-123.122478208265,183.423523407144,46.3038641989655));
#20822=CARTESIAN_POINT('Origin',(-107.170701202831,71.4826465587667,43.5630588771165));
#20823=CARTESIAN_POINT('',(-107.87121530948,184.586257960267,45.0000000000001));
#20824=CARTESIAN_POINT('Ctrl Pts',(-107.87121530948,184.586257960267,45.0000000000001));
#20825=CARTESIAN_POINT('Ctrl Pts',(-110.146583407099,184.571444762264,45.0000000000001));
#20826=CARTESIAN_POINT('Ctrl Pts',(-112.409195439908,184.486203531093,45.0865304305993));
#20827=CARTESIAN_POINT('Ctrl Pts',(-114.65936227692,184.332321719849,45.2572927923187));
#20828=CARTESIAN_POINT('Ctrl Pts',(-114.951570140632,184.312338545895,45.2794680835459));
#20829=CARTESIAN_POINT('Ctrl Pts',(-115.24356812522,184.291197789453,45.3030638979795));
#20830=CARTESIAN_POINT('Ctrl Pts',(-115.535356905797,184.268903325358,45.3280752522795));
#20831=CARTESIAN_POINT('Ctrl Pts',(-118.080214956822,184.074460460436,45.5462136818366));
#20832=CARTESIAN_POINT('Ctrl Pts',(-120.60917316356,183.792255035651,45.8720326958299));
#20833=CARTESIAN_POINT('Ctrl Pts',(-123.122478208265,183.423523407144,46.3038641989655));
#20834=CARTESIAN_POINT('Origin',(-107.155103814224,74.5885889652995,45.0000000000001));
#20835=CARTESIAN_POINT('Origin',(-107.155103814224,74.5885889652995,-44.9999999999999));
#20836=CARTESIAN_POINT('Origin',(-108.033967922038,-3.74818120714567E-13,
-180.));
#20837=CARTESIAN_POINT('',(-113.709994059637,250.,-70.1465397573417));
#20838=CARTESIAN_POINT('Origin',(-109.765188581367,199.3102738337,-146.488884695695));
#20839=CARTESIAN_POINT('Origin',(-108.033967922038,250.,-180.));
#20840=CARTESIAN_POINT('Ctrl Pts',(-108.033967922038,209.585728186396,-69.9999999999999));
#20841=CARTESIAN_POINT('Ctrl Pts',(-110.270464428139,209.567858930397,-69.9999999999999));
#20842=CARTESIAN_POINT('Ctrl Pts',(-112.494413985885,209.46648519935,-70.068117723223));
#20843=CARTESIAN_POINT('Ctrl Pts',(-114.706120670835,209.28373893618,-70.2025349187483));
#20844=CARTESIAN_POINT('Ctrl Pts',(-115.037057397657,209.256394690859,-70.2226477063157));
#20845=CARTESIAN_POINT('Ctrl Pts',(-115.367720010236,209.227228522798,-70.2442449343946));
#20846=CARTESIAN_POINT('Ctrl Pts',(-115.698109518352,209.19624749802,-70.2673205759029));
#20847=CARTESIAN_POINT('Ctrl Pts',(-118.243257051566,208.957585927807,-70.4450832185398));
#20848=CARTESIAN_POINT('Ctrl Pts',(-120.772211061871,208.611218684354,-70.7105850995704));
#20849=CARTESIAN_POINT('Ctrl Pts',(-123.285230820823,208.15873578029,-71.0624078658236));
#20850=CARTESIAN_POINT('Origin',(-40.3363668356791,225.625863228014,-34.2057557851748));
#20851=CARTESIAN_POINT('Origin',(-133.630782057879,206.966980183574,-47.2669739162828));
#20852=CARTESIAN_POINT('Ctrl Pts',(-123.122478208265,183.423523407144,-46.3038641989654));
#20853=CARTESIAN_POINT('Ctrl Pts',(-119.79626063639,183.911518935037,-70.573952040003));
#20854=CARTESIAN_POINT('Ctrl Pts',(-123.285230820823,208.15873578029,-71.0624078658236));
#20855=CARTESIAN_POINT('Ctrl Pts',(-124.998899886253,183.148230114533,-46.6262675599709));
#20856=CARTESIAN_POINT('Ctrl Pts',(-121.695019586639,183.691462295903,-70.8397782931125));
#20857=CARTESIAN_POINT('Ctrl Pts',(-125.588111971152,207.820875830254,-71.3848112268697));
#20858=CARTESIAN_POINT('Ctrl Pts',(-126.86819905826,182.824399215534,-46.9474471449936));
#20859=CARTESIAN_POINT('Ctrl Pts',(-123.591604529994,183.421472951449,-71.1053001850761));
#20860=CARTESIAN_POINT('Ctrl Pts',(-127.882251854971,207.423447001444,-71.7059908106043));
#20861=CARTESIAN_POINT('Ctrl Pts',(-128.727878679424,182.452463291301,-47.2669739162828));
#20862=CARTESIAN_POINT('Ctrl Pts',(-125.483223478439,183.101394331498,-71.3701268378898));
#20863=CARTESIAN_POINT('Ctrl Pts',(-130.164585944519,206.966980183574,-72.0255175831411));
#20864=CARTESIAN_POINT('Origin',(-126.751426934183,208.15873578029,-46.3038641989653));
#20865=CARTESIAN_POINT('Ctrl Pts',(-107.87121530948,184.586257960267,-44.9999999999999));
#20866=CARTESIAN_POINT('Ctrl Pts',(-107.87121530948,184.586257960267,-69.9999999999999));
#20867=CARTESIAN_POINT('Ctrl Pts',(-108.033967922038,209.585728186396,-69.9999999999999));
#20868=CARTESIAN_POINT('Ctrl Pts',(-110.438920857601,184.569541574581,-44.9999999999671));
#20869=CARTESIAN_POINT('Ctrl Pts',(-109.855167975854,184.573341947487,-69.9962013003749));
#20870=CARTESIAN_POINT('Ctrl Pts',(-110.601673611506,209.565212621119,-69.9999999999999));
#20871=CARTESIAN_POINT('Ctrl Pts',(-112.993544026661,184.463113520349,-45.1101978466298));
#20872=CARTESIAN_POINT('Ctrl Pts',(-111.8270421663,184.512020248025,-70.0409090864542));
#20873=CARTESIAN_POINT('Ctrl Pts',(-113.156296639219,209.434596373781,-70.0897908380047));
#20874=CARTESIAN_POINT('Ctrl Pts',(-118.077169784938,184.074693130366,-45.5459526578601));
#20875=CARTESIAN_POINT('Ctrl Pts',(-115.791831475917,184.289393680222,-70.2300552343412));
#20876=CARTESIAN_POINT('Ctrl Pts',(-118.239922397497,208.957898622415,-70.4448503138019));
#20877=CARTESIAN_POINT('Ctrl Pts',(-120.606185416306,183.792693373573,-45.8715193467126));
#20878=CARTESIAN_POINT('Ctrl Pts',(-117.778521014566,184.128732905586,-70.3739036491836));
#20879=CARTESIAN_POINT('Ctrl Pts',(-120.768938161273,208.611807987944,-70.7101268934865));
#20880=CARTESIAN_POINT('Ctrl Pts',(-123.122478208265,183.423523407144,-46.3038641989653));
#20881=CARTESIAN_POINT('Ctrl Pts',(-119.79626063639,183.911518935037,-70.573952040003));
#20882=CARTESIAN_POINT('Ctrl Pts',(-123.285230820823,208.15873578029,-71.0624078658236));
#20883=CARTESIAN_POINT('Origin',(-108.033967922038,209.585728186396,-44.9999999999999));
#20884=CARTESIAN_POINT('Origin',(-107.155103814224,74.5885889652995,-44.9999999999999));
#20885=CARTESIAN_POINT('Origin',(-93.0342906798268,208.848049102839,-45.));
#20886=CARTESIAN_POINT('Origin',(-115.,0.,-44.9999999999999));
#20887=CARTESIAN_POINT('Ctrl Pts',(-14.5652173913044,184.425742352699,-70.));
#20888=CARTESIAN_POINT('Ctrl Pts',(-16.3332090306658,184.754274466599,-70.));
#20889=CARTESIAN_POINT('Ctrl Pts',(-18.1023329015486,185.057744804456,-69.9814986316322));
#20890=CARTESIAN_POINT('Ctrl Pts',(-19.872512033359,185.336453963332,-69.9438574986233));
#20891=CARTESIAN_POINT('Ctrl Pts',(-21.6426911651695,185.615163122208,-69.9062163656144));
#20892=CARTESIAN_POINT('Ctrl Pts',(-23.413925616323,185.869111277598,-69.8494352575069));
#20893=CARTESIAN_POINT('Ctrl Pts',(-25.1861398363754,186.098646846334,-69.7729130408332));
#20894=CARTESIAN_POINT('Ctrl Pts',(-25.5781521525593,186.149419923837,-69.7559863899473));
#20895=CARTESIAN_POINT('Ctrl Pts',(-25.9702115289155,186.198996530262,-69.7380937641867));
#20896=CARTESIAN_POINT('Ctrl Pts',(-26.3623178779184,186.247381007943,-69.7192288310756));
#20897=CARTESIAN_POINT('Ctrl Pts',(-28.0897549408391,186.460540372048,-69.6361187648179));
#20898=CARTESIAN_POINT('Ctrl Pts',(-29.8181218381042,186.650553146811,-69.5341740687916));
#20899=CARTESIAN_POINT('Ctrl Pts',(-31.547298538853,186.817623039099,-69.4121562675502));
#20900=CARTESIAN_POINT('Ctrl Pts',(-32.9744695816452,186.955513696713,-69.3114492243883));
#20901=CARTESIAN_POINT('Ctrl Pts',(-34.4021922929087,187.077776406133,-69.1970689821003));
#20902=CARTESIAN_POINT('Ctrl Pts',(-35.8304007809344,187.184542684468,-69.068339898143));
#20903=CARTESIAN_POINT('Ctrl Pts',(-36.6176289651215,187.243392232087,-68.9973844572074));
#20904=CARTESIAN_POINT('Ctrl Pts',(-37.4050006589494,187.297524969372,-68.922068073687));
#20905=CARTESIAN_POINT('Ctrl Pts',(-38.1925161207239,187.346963461637,-68.8422776054607));
#20906=CARTESIAN_POINT('Ctrl Pts',(-40.0459152858722,187.463315793415,-68.6544926102758));
#20907=CARTESIAN_POINT('Ctrl Pts',(-41.9000878550032,187.553637649455,-68.4417940850099));
#20908=CARTESIAN_POINT('Ctrl Pts',(-43.7548464440809,187.618108571057,-68.2017594754763));
#20909=CARTESIAN_POINT('Ctrl Pts',(-43.8781086657332,187.62239313352,-68.1858074268276));
#20910=CARTESIAN_POINT('Ctrl Pts',(-44.0013734754008,187.62656353256,-68.1697346633771));
#20911=CARTESIAN_POINT('Ctrl Pts',(-44.1246408180115,187.630619824725,-68.1535404814305));
#20912=CARTESIAN_POINT('Ctrl Pts',(-44.9138902588186,187.656591231711,-68.0498532535323));
#20913=CARTESIAN_POINT('Ctrl Pts',(-45.7032416288397,187.677883839451,-67.9411788907505));
#20914=CARTESIAN_POINT('Ctrl Pts',(-46.492669161194,187.694509338513,-67.8272800457684));
#20915=CARTESIAN_POINT('Ctrl Pts',(-46.6935155796415,187.69873920358,-67.7983018632978));
#20916=CARTESIAN_POINT('Ctrl Pts',(-46.8943739810412,187.702667120824,-67.7689845079355));
#20917=CARTESIAN_POINT('Ctrl Pts',(-47.0952639568852,187.706293513407,-67.7393209875906));
#20918=CARTESIAN_POINT('Ctrl Pts',(-47.747314955179,187.718064100236,-67.6430387914656));
#20919=CARTESIAN_POINT('Ctrl Pts',(-48.3997417071708,187.726644621486,-67.5430866920454));
#20920=CARTESIAN_POINT('Ctrl Pts',(-49.051045556932,187.732055009666,-67.4395736529904));
#20921=CARTESIAN_POINT('Ctrl Pts',(-49.3882561779941,187.734856221971,-67.3859800864844));
#20922=CARTESIAN_POINT('Ctrl Pts',(-49.7251654725643,187.736807214015,-67.331431509529));
#20923=CARTESIAN_POINT('Ctrl Pts',(-50.0615611195167,187.737908013141,-67.2759403248462));
#20924=CARTESIAN_POINT('Ctrl Pts',(-50.6474554155661,187.739825255337,-67.1792923186035));
#20925=CARTESIAN_POINT('Ctrl Pts',(-51.2324498655741,187.739178946069,-67.0796996497906));
#20926=CARTESIAN_POINT('Ctrl Pts',(-51.8169655883217,187.735991706155,-66.9769680882559));
#20927=CARTESIAN_POINT('Ctrl Pts',(-52.8892222062581,187.730144918877,-66.7885136251172));
#20928=CARTESIAN_POINT('Ctrl Pts',(-53.958658043911,187.715757546733,-66.589710153915));
#20929=CARTESIAN_POINT('Ctrl Pts',(-55.025126049737,187.692983980761,-66.3798156662999));
#20930=CARTESIAN_POINT('Ctrl Pts',(-55.3182459502838,187.686724641188,-66.3221259362761));
#20931=CARTESIAN_POINT('Ctrl Pts',(-55.6111414887107,187.679831757017,-66.2635981034966));
#20932=CARTESIAN_POINT('Ctrl Pts',(-55.9038092350969,187.67230848245,-66.2042161775242));
#20933=CARTESIAN_POINT('Ctrl Pts',(-56.3020859570986,187.662070438901,-66.123406320222));
#20934=CARTESIAN_POINT('Ctrl Pts',(-56.6999420224511,187.650664478993,-66.0410161314753));
#20935=CARTESIAN_POINT('Ctrl Pts',(-57.0973581429572,187.638100024657,-65.9569932475349));
#20936=CARTESIAN_POINT('Ctrl Pts',(-57.9831815087046,187.610094398679,-65.7697098686999));
#20937=CARTESIAN_POINT('Ctrl Pts',(-58.8667491346833,187.576343097077,-65.5743373152664));
#20938=CARTESIAN_POINT('Ctrl Pts',(-59.748022636317,187.536944885931,-65.3702357907628));
#20939=CARTESIAN_POINT('Ctrl Pts',(-60.3701587719641,187.509131669276,-65.226150063121));
#20940=CARTESIAN_POINT('Ctrl Pts',(-60.9911510499064,187.478503994181,-65.0777132914352));
#20941=CARTESIAN_POINT('Ctrl Pts',(-61.6109773508216,187.445093862065,-64.9246875207813));
#20942=CARTESIAN_POINT('Ctrl Pts',(-62.4246579959206,187.401234513386,-64.7238020346402));
#20943=CARTESIAN_POINT('Ctrl Pts',(-63.2363399885754,187.352576836396,-64.5150207754862));
#20944=CARTESIAN_POINT('Ctrl Pts',(-64.0458122363587,187.299219962311,-64.2976170779646));
#20945=CARTESIAN_POINT('Ctrl Pts',(-64.8354194022501,187.247172507637,-64.0855486371695));
#20946=CARTESIAN_POINT('Ctrl Pts',(-65.6229240187697,187.190653571721,-63.8652758490625));
#20947=CARTESIAN_POINT('Ctrl Pts',(-66.4081014307383,187.129752250111,-63.6360837689149));
#20948=CARTESIAN_POINT('Ctrl Pts',(-66.6607827592823,187.110153333204,-63.5623264773516));
#20949=CARTESIAN_POINT('Ctrl Pts',(-66.9132228410625,187.090100539921,-63.4876451395221));
#20950=CARTESIAN_POINT('Ctrl Pts',(-67.1654135146365,187.06959679849,-63.4120149817037));
#20951=CARTESIAN_POINT('Ctrl Pts',(-67.2763479110417,187.060577550682,-63.3787465590903));
#20952=CARTESIAN_POINT('Ctrl Pts',(-67.3872335922792,187.051471155586,-63.3452940284817));
#20953=CARTESIAN_POINT('Ctrl Pts',(-67.4980694122349,187.042277973773,-63.3116547642332));
#20954=CARTESIAN_POINT('Ctrl Pts',(-68.1891623934665,186.984955860499,-63.1019043475792));
#20955=CARTESIAN_POINT('Ctrl Pts',(-68.8784061259738,186.92425066319,-62.8848692013738));
#20956=CARTESIAN_POINT('Ctrl Pts',(-69.5656014077318,186.860244783527,-62.6598608171745));
#20957=CARTESIAN_POINT('Ctrl Pts',(-69.6694849243805,186.85056899552,-62.6258462323156));
#20958=CARTESIAN_POINT('Ctrl Pts',(-69.7733215727291,186.840817773274,-62.591649360303));
#20959=CARTESIAN_POINT('Ctrl Pts',(-69.8771106036008,186.83099139587,-62.5572677367493));
#20960=CARTESIAN_POINT('Ctrl Pts',(-69.9376320137037,186.825261443372,-62.5372191408464));
#20961=CARTESIAN_POINT('Ctrl Pts',(-69.9981396362794,186.819505511523,-62.5171063931954));
#20962=CARTESIAN_POINT('Ctrl Pts',(-70.0586302384664,186.813724031626,-62.4969301244232));
#20963=CARTESIAN_POINT('Ctrl Pts',(-70.4373401605021,186.777528263659,-62.3706137563026));
#20964=CARTESIAN_POINT('Ctrl Pts',(-70.8154187338308,186.740326306256,-62.2417960880244));
#20965=CARTESIAN_POINT('Ctrl Pts',(-71.1924802640547,186.70217904041,-62.1104779549871));
#20966=CARTESIAN_POINT('Ctrl Pts',(-71.5383672842266,186.66718569568,-61.9900168787701));
#20967=CARTESIAN_POINT('Ctrl Pts',(-71.883398906256,186.631396708284,-61.8674513360236));
#20968=CARTESIAN_POINT('Ctrl Pts',(-72.22723352361,186.594856854709,-61.7427730099849));
#20969=CARTESIAN_POINT('Ctrl Pts',(-72.3285124818555,186.584093778166,-61.7060481127824));
#20970=CARTESIAN_POINT('Ctrl Pts',(-72.4296872512436,186.573265547093,-61.6691398576058));
#20971=CARTESIAN_POINT('Ctrl Pts',(-72.53074821145,186.562373297712,-61.6320479328138));
#20972=CARTESIAN_POINT('Ctrl Pts',(-72.5524850931717,186.560030518304,-61.624069948235));
#20973=CARTESIAN_POINT('Ctrl Pts',(-72.5742182031628,186.557684636607,-61.6160830365718));
#20974=CARTESIAN_POINT('Ctrl Pts',(-72.5959475943732,186.555335651049,-61.6080871405041));
#20975=CARTESIAN_POINT('Ctrl Pts',(-73.0750811308316,186.503540469726,-61.4317774628443));
#20976=CARTESIAN_POINT('Ctrl Pts',(-73.5520260771487,186.450278236732,-61.2512439961753));
#20977=CARTESIAN_POINT('Ctrl Pts',(-74.0266639966632,186.39561293057,-61.0661252075006));
#20978=CARTESIAN_POINT('Ctrl Pts',(-74.4933003459508,186.341869186442,-60.8841271997981));
#20979=CARTESIAN_POINT('Ctrl Pts',(-74.9577069279405,186.286769176235,-60.6976972459528));
#20980=CARTESIAN_POINT('Ctrl Pts',(-75.4197294652055,186.230378252862,-60.5064652710687));
#20981=CARTESIAN_POINT('Ctrl Pts',(-75.870278313599,186.175387719854,-60.3199822770354));
#20982=CARTESIAN_POINT('Ctrl Pts',(-76.3185601193047,186.119169509541,-60.1289328394813));
#20983=CARTESIAN_POINT('Ctrl Pts',(-76.7643904712269,186.061789933078,-59.9329475682572));
#20984=CARTESIAN_POINT('Ctrl Pts',(-77.0251398082259,186.028230785622,-59.8183231840874));
#20985=CARTESIAN_POINT('Ctrl Pts',(-77.285049808661,185.994274490326,-59.7020099337784));
#20986=CARTESIAN_POINT('Ctrl Pts',(-77.5440766099974,185.959935431812,-59.5839295084219));
#20987=CARTESIAN_POINT('Ctrl Pts',(-77.5450711085164,185.959803591622,-59.5834761545314));
#20988=CARTESIAN_POINT('Ctrl Pts',(-77.5460655939007,185.959671745816,-59.5830227745252));
#20989=CARTESIAN_POINT('Ctrl Pts',(-77.5470600661468,185.959539894396,-59.582569368398));
#20990=CARTESIAN_POINT('Ctrl Pts',(-77.9410693805506,185.907300440083,-59.4029301295733));
#20991=CARTESIAN_POINT('Ctrl Pts',(-78.332979228556,185.85418497661,-59.2192124213913));
#20992=CARTESIAN_POINT('Ctrl Pts',(-78.7227006320066,185.800243549814,-59.0310068937098));
#20993=CARTESIAN_POINT('Ctrl Pts',(-79.0870092104663,185.749819517821,-58.8550738101255));
#20994=CARTESIAN_POINT('Ctrl Pts',(-79.4494052396861,185.698673675177,-58.6752189694766));
#20995=CARTESIAN_POINT('Ctrl Pts',(-79.8097729729191,185.646852044688,-58.4910808942653));
#20996=CARTESIAN_POINT('Ctrl Pts',(-79.8349108990578,185.64323715856,-58.4782361001644));
#20997=CARTESIAN_POINT('Ctrl Pts',(-79.860038937817,185.639618986481,-58.4653704529016));
#20998=CARTESIAN_POINT('Ctrl Pts',(-79.8851570418036,185.635997545186,-58.4524838246918));
#20999=CARTESIAN_POINT('Ctrl Pts',(-80.2271667926614,185.586687763051,-58.2770186500199));
#21000=CARTESIAN_POINT('Ctrl Pts',(-80.5673404844472,185.536770724644,-58.097667248913));
#21001=CARTESIAN_POINT('Ctrl Pts',(-80.905487185369,185.486304601332,-57.9140644289558));
#21002=CARTESIAN_POINT('Ctrl Pts',(-81.2350552092114,185.43711878794,-57.7351195556797));
#21003=CARTESIAN_POINT('Ctrl Pts',(-81.5626978743657,185.387411331872,-57.552136292134));
#21004=CARTESIAN_POINT('Ctrl Pts',(-81.8881965724081,185.337243380279,-57.3647505333222));
#21005=CARTESIAN_POINT('Ctrl Pts',(-81.9594892979342,185.326255287163,-57.3237081526589));
#21006=CARTESIAN_POINT('Ctrl Pts',(-82.030679006116,185.315245133469,-57.2824544704765));
#21007=CARTESIAN_POINT('Ctrl Pts',(-82.1017631156658,185.304213614831,-57.2409854846495));
#21008=CARTESIAN_POINT('Ctrl Pts',(-82.1641085977492,185.294538240799,-57.2046144316918));
#21009=CARTESIAN_POINT('Ctrl Pts',(-82.2263725660917,185.284846503345,-57.1680775913122));
#21010=CARTESIAN_POINT('Ctrl Pts',(-82.2885528589849,185.275138973569,-57.1313720132604));
#21011=CARTESIAN_POINT('Ctrl Pts',(-82.5537094566501,185.233742970956,-56.9748477233497));
#21012=CARTESIAN_POINT('Ctrl Pts',(-82.8173085533163,185.192065700995,-56.815280772334));
#21013=CARTESIAN_POINT('Ctrl Pts',(-83.0793493574573,185.15012491829,-56.6523178031346));
#21014=CARTESIAN_POINT('Ctrl Pts',(-83.1059294390114,185.145870659384,-56.6357876714026));
#21015=CARTESIAN_POINT('Ctrl Pts',(-83.1324934497333,185.141613693795,-56.6192225744983));
#21016=CARTESIAN_POINT('Ctrl Pts',(-83.1590413630191,185.137354043298,-56.6026221275495));
#21017=CARTESIAN_POINT('Ctrl Pts',(-83.3477570764781,185.107074338296,-56.4846179305355));
#21018=CARTESIAN_POINT('Ctrl Pts',(-83.5358233772913,185.076631188317,-56.3647122352436));
#21019=CARTESIAN_POINT('Ctrl Pts',(-83.7227350501772,185.04611606651,-56.2430899760604));
#21020=CARTESIAN_POINT('Ctrl Pts',(-83.8754267602103,185.021187681574,-56.1437344331665));
#21021=CARTESIAN_POINT('Ctrl Pts',(-84.0273472610658,184.996211366635,-56.0432334924026));
#21022=CARTESIAN_POINT('Ctrl Pts',(-84.1781966533824,184.971240983028,-55.941695692402));
#21023=CARTESIAN_POINT('Ctrl Pts',(-84.3028452567794,184.950607665286,-55.8577938299702));
#21024=CARTESIAN_POINT('Ctrl Pts',(-84.4268258047856,184.929968681078,-55.7731493348459));
#21025=CARTESIAN_POINT('Ctrl Pts',(-84.550121873792,184.90933042457,-55.6877257199939));
#21026=CARTESIAN_POINT('Ctrl Pts',(-84.7876740654026,184.869567088205,-55.5231416656365));
#21027=CARTESIAN_POINT('Ctrl Pts',(-85.0226597642961,184.829811900678,-55.35568886156));
#21028=CARTESIAN_POINT('Ctrl Pts',(-85.2549076799668,184.790120644856,-55.1851091265834));
#21029=CARTESIAN_POINT('Ctrl Pts',(-85.4820939782465,184.751294421344,-55.0182470109903));
#21030=CARTESIAN_POINT('Ctrl Pts',(-85.7066606083177,184.712529308532,-54.8483927990932));
#21031=CARTESIAN_POINT('Ctrl Pts',(-85.9284004963375,184.673887791977,-54.6752898962077));
#21032=CARTESIAN_POINT('Ctrl Pts',(-85.9743358203938,184.665882869629,-54.6394301417443));
#21033=CARTESIAN_POINT('Ctrl Pts',(-86.0201496699684,184.657883289184,-54.60343091788));
#21034=CARTESIAN_POINT('Ctrl Pts',(-86.0658399404311,184.64988966699,-54.5672898593966));
#21035=CARTESIAN_POINT('Ctrl Pts',(-86.2709553449911,184.614004235942,-54.405043329512));
#21036=CARTESIAN_POINT('Ctrl Pts',(-86.4735852521456,184.578237776751,-54.2399399631925));
#21037=CARTESIAN_POINT('Ctrl Pts',(-86.6734831582947,184.542656686666,-54.0717480448259));
#21038=CARTESIAN_POINT('Ctrl Pts',(-86.8570706538062,184.509978789523,-53.9172795281064));
#21039=CARTESIAN_POINT('Ctrl Pts',(-87.0383425977796,184.477460157983,-53.7602184288664));
#21040=CARTESIAN_POINT('Ctrl Pts',(-87.2171464938128,184.445147523806,-53.6003097299749));
#21041=CARTESIAN_POINT('Ctrl Pts',(-87.3923292574055,184.413489284362,-53.4436394984206));
#21042=CARTESIAN_POINT('Ctrl Pts',(-87.5651430323094,184.382028724284,-53.2842358707506));
#21043=CARTESIAN_POINT('Ctrl Pts',(-87.7353991285702,184.350819525833,-53.1218444821961));
#21044=CARTESIAN_POINT('Ctrl Pts',(-87.8984589116787,184.320929464671,-52.9663169846326));
#21045=CARTESIAN_POINT('Ctrl Pts',(-88.0591750208179,184.291269544404,-52.8080497256244));
#21046=CARTESIAN_POINT('Ctrl Pts',(-88.2173066844818,184.261901670574,-52.6467953084342));
#21047=CARTESIAN_POINT('Ctrl Pts',(-88.3489258435748,184.237457642298,-52.51257695963));
#21048=CARTESIAN_POINT('Ctrl Pts',(-88.478753822866,184.213216087887,-52.3762889160388));
#21049=CARTESIAN_POINT('Ctrl Pts',(-88.6066260845763,184.189218592662,-52.2377803000698));
#21050=CARTESIAN_POINT('Ctrl Pts',(-88.7423987435818,184.163738447926,-52.0907141354948));
#21051=CARTESIAN_POINT('Ctrl Pts',(-88.8759595521882,184.138535045677,-51.9411553279166));
#21052=CARTESIAN_POINT('Ctrl Pts',(-89.007139024002,184.113653620594,-51.7888395413096));
#21053=CARTESIAN_POINT('Ctrl Pts',(-89.0610951115254,184.103419516653,-51.7261897699718));
#21054=CARTESIAN_POINT('Ctrl Pts',(-89.1146477662933,184.093240005199,-51.6630733955921));
#21055=CARTESIAN_POINT('Ctrl Pts',(-89.1677827797996,184.083118761996,-51.5994712579033));
#21056=CARTESIAN_POINT('Ctrl Pts',(-89.2735870907887,184.062964985931,-51.4728244404557));
#21057=CARTESIAN_POINT('Ctrl Pts',(-89.3778592759144,184.043017998514,-51.3440714967514));
#21058=CARTESIAN_POINT('Ctrl Pts',(-89.4802240523979,184.02335791968,-51.2133748814786));
#21059=CARTESIAN_POINT('Ctrl Pts',(-89.5846662384106,184.003298855603,-51.0800258851492));
#21060=CARTESIAN_POINT('Ctrl Pts',(-89.6871213991053,183.983539255981,-50.9446550233047));
#21061=CARTESIAN_POINT('Ctrl Pts',(-89.787050816559,183.964192805037,-50.8075906059771));
#21062=CARTESIAN_POINT('Ctrl Pts',(-89.9538329812593,183.931903584806,-50.5788301387615));
#21063=CARTESIAN_POINT('Ctrl Pts',(-90.1134653217683,183.900788683591,-50.3455986429249));
#21064=CARTESIAN_POINT('Ctrl Pts',(-90.2649122865753,183.871104542861,-50.107908393505));
#21065=CARTESIAN_POINT('Ctrl Pts',(-90.2869520658823,183.866784668168,-50.0733177983925));
#21066=CARTESIAN_POINT('Ctrl Pts',(-90.3088215648408,183.86249445937,-50.0386276981052));
#21067=CARTESIAN_POINT('Ctrl Pts',(-90.3305184659637,183.858234565329,-50.0038364107849));
#21068=CARTESIAN_POINT('Ctrl Pts',(-90.4388801877854,183.836959202068,-49.830076859729));
#21069=CARTESIAN_POINT('Ctrl Pts',(-90.5429465739695,183.816439370396,-49.653794440825));
#21070=CARTESIAN_POINT('Ctrl Pts',(-90.6423754682554,183.796762200223,-49.4747737442102));
#21071=CARTESIAN_POINT('Ctrl Pts',(-90.7359515882384,183.778243305386,-49.306290907242));
#21072=CARTESIAN_POINT('Ctrl Pts',(-90.8254198130981,183.760470832419,-49.1353826443591));
#21073=CARTESIAN_POINT('Ctrl Pts',(-90.9104447973024,183.74352951109,-48.9618638325262));
#21074=CARTESIAN_POINT('Ctrl Pts',(-90.9157627357116,183.742469906032,-48.9510109948243));
#21075=CARTESIAN_POINT('Ctrl Pts',(-90.9210632759633,183.741413556434,-48.9401479429578));
#21076=CARTESIAN_POINT('Ctrl Pts',(-90.9263463293841,183.740360484662,-48.9292746308957));
#21077=CARTESIAN_POINT('Ctrl Pts',(-90.9852403645883,183.72862112845,-48.8080619206772));
#21078=CARTESIAN_POINT('Ctrl Pts',(-91.0421061938172,183.717259001773,-48.6852599408307));
#21079=CARTESIAN_POINT('Ctrl Pts',(-91.0966291024536,183.706343449781,-48.5611616805563));
#21080=CARTESIAN_POINT('Ctrl Pts',(-91.1243382887326,183.700796037307,-48.4980934786416));
#21081=CARTESIAN_POINT('Ctrl Pts',(-91.1514431441962,183.695363828463,-48.4346905584647));
#21082=CARTESIAN_POINT('Ctrl Pts',(-91.1779074466647,183.690055029156,-48.3709919142252));
#21083=CARTESIAN_POINT('Ctrl Pts',(-91.2289358904181,183.679818607202,-48.2481682468109));
#21084=CARTESIAN_POINT('Ctrl Pts',(-91.2775802069475,183.670041568329,-48.1242448232095));
#21085=CARTESIAN_POINT('Ctrl Pts',(-91.3236087361308,183.660775010778,-47.9995040966891));
#21086=CARTESIAN_POINT('Ctrl Pts',(-91.3642312992659,183.652596793359,-47.8894139389433));
#21087=CARTESIAN_POINT('Ctrl Pts',(-91.4028170594171,183.644816079972,-47.778687252021));
#21088=CARTESIAN_POINT('Ctrl Pts',(-91.4392397760242,183.637461709821,-47.6675216693592));
#21089=CARTESIAN_POINT('Ctrl Pts',(-91.5301427046272,183.619106852,-47.3900773169012));
#21090=CARTESIAN_POINT('Ctrl Pts',(-91.6075721796016,183.603408457479,-47.1099727365793));
#21091=CARTESIAN_POINT('Ctrl Pts',(-91.6708671314707,183.590553705567,-46.8270612872151));
#21092=CARTESIAN_POINT('Ctrl Pts',(-91.6800654005284,183.588685602926,-46.7859474929247));
#21093=CARTESIAN_POINT('Ctrl Pts',(-91.6889650755193,183.586877577863,-46.744774411718));
#21094=CARTESIAN_POINT('Ctrl Pts',(-91.6975640385099,183.585130228127,-46.7035415847502));
#21095=CARTESIAN_POINT('Ctrl Pts',(-91.7555966293713,183.573337732632,-46.4252699163973));
#21096=CARTESIAN_POINT('Ctrl Pts',(-91.7999412124509,183.56430768583,-46.1442769510425));
#21097=CARTESIAN_POINT('Ctrl Pts',(-91.8297919983774,183.558222566852,-45.8604063906217));
#21098=CARTESIAN_POINT('Ctrl Pts',(-91.8596427843038,183.552137447875,-45.576535830201));
#21099=CARTESIAN_POINT('Ctrl Pts',(-91.8749999999089,183.548997205095,-45.2897876967856));
#21100=CARTESIAN_POINT('Ctrl Pts',(-91.875,183.548997205106,-45.));
#21101=CARTESIAN_POINT('Origin',(-40.3363668356791,225.625863228014,34.2057557851749));
#21102=CARTESIAN_POINT('Origin',(-133.630782057879,206.966980183574,47.2669739162829));
#21103=CARTESIAN_POINT('Ctrl Pts',(-128.727878679424,182.452463291301,47.2669739162829));
#21104=CARTESIAN_POINT('Ctrl Pts',(-125.483223478439,183.101394331498,71.37012683789));
#21105=CARTESIAN_POINT('Ctrl Pts',(-130.164585944519,206.966980183574,72.0255175831412));
#21106=CARTESIAN_POINT('Ctrl Pts',(-126.868199058258,182.824399215534,46.9474471450068));
#21107=CARTESIAN_POINT('Ctrl Pts',(-123.591604530024,183.421472951552,71.1053001850989));
#21108=CARTESIAN_POINT('Ctrl Pts',(-127.882251854987,207.423447001473,71.7059908106067));
#21109=CARTESIAN_POINT('Ctrl Pts',(-124.998899886252,183.148230114533,46.626267559976));
#21110=CARTESIAN_POINT('Ctrl Pts',(-121.695019586642,183.691462296002,70.8397782930618));
#21111=CARTESIAN_POINT('Ctrl Pts',(-125.588111971157,207.820875830351,71.3848112268705));
#21112=CARTESIAN_POINT('Ctrl Pts',(-123.122478208265,183.423523407144,46.3038641989655));
#21113=CARTESIAN_POINT('Ctrl Pts',(-119.79626063639,183.911518935037,70.5739520400031));
#21114=CARTESIAN_POINT('Ctrl Pts',(-123.285230820823,208.15873578029,71.0624078658238));
#21115=CARTESIAN_POINT('Origin',(-126.751426934183,208.15873578029,46.3038641989655));
#21116=CARTESIAN_POINT('Ctrl Pts',(-108.033967922038,209.585728186396,70.));
#21117=CARTESIAN_POINT('Ctrl Pts',(-107.87121530948,184.586257960267,70.));
#21118=CARTESIAN_POINT('Ctrl Pts',(-107.87121530948,184.586257960267,45.));
#21119=CARTESIAN_POINT('Ctrl Pts',(-110.601673611534,209.565212621119,70.));
#21120=CARTESIAN_POINT('Ctrl Pts',(-109.85516797587,184.573341947487,69.9962013003751));
#21121=CARTESIAN_POINT('Ctrl Pts',(-110.438920857634,184.569541574581,44.9999999999672));
#21122=CARTESIAN_POINT('Ctrl Pts',(-113.15629663918,209.434596373781,70.0897908380021));
#21123=CARTESIAN_POINT('Ctrl Pts',(-111.827042166278,184.512020248025,70.0409090865197));
#21124=CARTESIAN_POINT('Ctrl Pts',(-112.993544026618,184.463113520352,45.1101978466734));
#21125=CARTESIAN_POINT('Ctrl Pts',(-118.239922397535,208.957898622415,70.4448503138047));
#21126=CARTESIAN_POINT('Ctrl Pts',(-115.791831475939,184.289393680222,70.2300552342761));
#21127=CARTESIAN_POINT('Ctrl Pts',(-118.077169784981,184.074693130363,45.5459526578167));
#21128=CARTESIAN_POINT('Ctrl Pts',(-120.768938161246,208.611807987957,70.7101268934829));
#21129=CARTESIAN_POINT('Ctrl Pts',(-117.778521014579,184.128732905726,70.3739036490886));
#21130=CARTESIAN_POINT('Ctrl Pts',(-120.606185416313,183.792693373572,45.8715193465168));
#21131=CARTESIAN_POINT('Ctrl Pts',(-123.285230820823,208.15873578029,71.0624078658237));
#21132=CARTESIAN_POINT('Ctrl Pts',(-119.79626063639,183.911518935037,70.5739520400031));
#21133=CARTESIAN_POINT('Ctrl Pts',(-123.122478208265,183.423523407144,46.3038641989654));
#21134=CARTESIAN_POINT('Origin',(-108.033967922038,209.585728186396,45.0000000000001));
#21135=CARTESIAN_POINT('Origin',(-107.155103814224,74.5885889652995,45.0000000000001));
#21136=CARTESIAN_POINT('Origin',(-93.0342906798268,208.848049102839,45.0000000000001));
#21137=CARTESIAN_POINT('Origin',(-115.,0.,45.0000000000001));
#21138=CARTESIAN_POINT('Ctrl Pts',(-91.875,183.548997205106,45.0000000000001));
#21139=CARTESIAN_POINT('Ctrl Pts',(-91.8749999998576,183.548997205088,45.2896000759332));
#21140=CARTESIAN_POINT('Ctrl Pts',(-91.8596625980027,183.552133377192,45.5762242871697));
#21141=CARTESIAN_POINT('Ctrl Pts',(-91.8298318968589,183.558214394318,45.8600283115351));
#21142=CARTESIAN_POINT('Ctrl Pts',(-91.8000011957152,183.564295411445,46.1438323359004));
#21143=CARTESIAN_POINT('Ctrl Pts',(-91.7556769885713,183.573321320276,46.4248161529088));
#21144=CARTESIAN_POINT('Ctrl Pts',(-91.6976496523008,183.585112765732,46.7031300609794));
#21145=CARTESIAN_POINT('Ctrl Pts',(-91.637369668756,183.5973619604,46.9922482400498));
#21146=CARTESIAN_POINT('Ctrl Pts',(-91.5622974063693,183.61259559088,47.2784857624134));
#21147=CARTESIAN_POINT('Ctrl Pts',(-91.473124343595,183.630616797189,47.561991552747));
#21148=CARTESIAN_POINT('Ctrl Pts',(-91.4617400188155,183.632917483733,47.598185464828));
#21149=CARTESIAN_POINT('Ctrl Pts',(-91.4501258054148,183.635263621029,47.6343348470904));
#21150=CARTESIAN_POINT('Ctrl Pts',(-91.4382830838388,183.63765481468,47.6704400035409));
#21151=CARTESIAN_POINT('Ctrl Pts',(-91.4056950676103,183.644234742865,47.7697917798027));
#21152=CARTESIAN_POINT('Ctrl Pts',(-91.3713189504872,183.651167837988,47.8689747154106));
#21153=CARTESIAN_POINT('Ctrl Pts',(-91.3353086631554,183.658420153658,47.9676327090243));
#21154=CARTESIAN_POINT('Ctrl Pts',(-91.2989262398865,183.665747415892,48.0673102497624));
#21155=CARTESIAN_POINT('Ctrl Pts',(-91.2608757374785,183.673400509824,48.1664519468418));
#21156=CARTESIAN_POINT('Ctrl Pts',(-91.2213678244624,183.681334352256,48.2646960569366));
#21157=CARTESIAN_POINT('Ctrl Pts',(-91.2150232933313,183.682608439051,48.2804729676201));
#21158=CARTESIAN_POINT('Ctrl Pts',(-91.2086412839471,183.683889745562,48.2962267419502));
#21159=CARTESIAN_POINT('Ctrl Pts',(-91.2022227901124,183.685178061878,48.3119558946997));
#21160=CARTESIAN_POINT('Ctrl Pts',(-91.1943916959767,183.686749914498,48.3311467639331));
#21161=CARTESIAN_POINT('Ctrl Pts',(-91.1865048506322,183.688332493241,48.3503045398201));
#21162=CARTESIAN_POINT('Ctrl Pts',(-91.1785628076855,183.689925674695,48.3694295168963));
#21163=CARTESIAN_POINT('Ctrl Pts',(-91.1087363643921,183.703932926374,48.5375763194571));
#21164=CARTESIAN_POINT('Ctrl Pts',(-91.034646476792,183.718758774971,48.7031880996127));
#21165=CARTESIAN_POINT('Ctrl Pts',(-90.9566165291512,183.734324372969,48.8664595502886));
#21166=CARTESIAN_POINT('Ctrl Pts',(-90.9461168373726,183.73641887625,48.8884293190783));
#21167=CARTESIAN_POINT('Ctrl Pts',(-90.9355457310213,183.738526792029,48.9103567058832));
#21168=CARTESIAN_POINT('Ctrl Pts',(-90.9249039291036,183.7406479451,48.932242178386));
#21169=CARTESIAN_POINT('Ctrl Pts',(-90.8406028436605,183.757451068078,49.1056121679495));
#21170=CARTESIAN_POINT('Ctrl Pts',(-90.7518683910998,183.775084743858,49.2763588350715));
#21171=CARTESIAN_POINT('Ctrl Pts',(-90.6590379490552,183.793463886533,49.4446683780763));
#21172=CARTESIAN_POINT('Ctrl Pts',(-90.5646175021781,183.812157828158,49.6158607360375));
#21173=CARTESIAN_POINT('Ctrl Pts',(-90.4659594745685,183.831623035935,49.7845317587114));
#21174=CARTESIAN_POINT('Ctrl Pts',(-90.3633670717736,183.85178248117,49.9508715143199));
#21175=CARTESIAN_POINT('Ctrl Pts',(-90.3531584694818,183.85378847531,49.9674233872078));
#21176=CARTESIAN_POINT('Ctrl Pts',(-90.3429108698052,183.85580135319,49.9839521723536));
#21177=CARTESIAN_POINT('Ctrl Pts',(-90.33262454449,183.857821045285,50.0004580539773));
#21178=CARTESIAN_POINT('Ctrl Pts',(-90.3098775310987,183.862287359708,50.0369588935699));
#21179=CARTESIAN_POINT('Ctrl Pts',(-90.2869409228782,183.866786973872,50.073347705516));
#21180=CARTESIAN_POINT('Ctrl Pts',(-90.2638174075046,183.871319137022,50.1096264538567));
#21181=CARTESIAN_POINT('Ctrl Pts',(-90.1478268110307,183.894053063871,50.2916054302969));
#21182=CARTESIAN_POINT('Ctrl Pts',(-90.0271359963355,183.917606706893,50.4708248827606));
#21183=CARTESIAN_POINT('Ctrl Pts',(-89.902092931984,183.941887340518,50.6474690155926));
#21184=CARTESIAN_POINT('Ctrl Pts',(-89.8652183685416,183.949047575831,50.6995604715772));
#21185=CARTESIAN_POINT('Ctrl Pts',(-89.8279649867759,183.956271120596,50.7514279342131));
#21186=CARTESIAN_POINT('Ctrl Pts',(-89.790340884684,183.963555813154,50.8030760387775));
#21187=CARTESIAN_POINT('Ctrl Pts',(-89.6982015750568,183.981395615459,50.9295593415947));
#21188=CARTESIAN_POINT('Ctrl Pts',(-89.6037507212967,183.999618439847,51.0548132891789));
#21189=CARTESIAN_POINT('Ctrl Pts',(-89.5074065290439,184.018135337854,51.1785589171201));
#21190=CARTESIAN_POINT('Ctrl Pts',(-89.4981849683562,184.019907678197,51.1904031994915));
#21191=CARTESIAN_POINT('Ctrl Pts',(-89.4889460311051,184.021682719221,51.2022336866468));
#21192=CARTESIAN_POINT('Ctrl Pts',(-89.4796900645198,184.023460387051,51.2140501483047));
#21193=CARTESIAN_POINT('Ctrl Pts',(-89.3862338429122,184.041409254643,51.3333593365078));
#21194=CARTESIAN_POINT('Ctrl Pts',(-89.2911914529099,184.059596578161,51.4510479915178));
#21195=CARTESIAN_POINT('Ctrl Pts',(-89.1948816910292,184.077954977797,51.5669472071899));
#21196=CARTESIAN_POINT('Ctrl Pts',(-89.1870865088545,184.079440881892,51.5763279333222));
#21197=CARTESIAN_POINT('Ctrl Pts',(-89.1792830000548,184.08092791161,51.5856969503268));
#21198=CARTESIAN_POINT('Ctrl Pts',(-89.1714713212156,184.082416033757,51.5950541756226));
#21199=CARTESIAN_POINT('Ctrl Pts',(-89.0488267301808,184.105779786404,51.7419640900277));
#21200=CARTESIAN_POINT('Ctrl Pts',(-88.9240271148734,184.129440547651,51.8861994560237));
#21201=CARTESIAN_POINT('Ctrl Pts',(-88.7972002069489,184.153362762024,52.0280454940487));
#21202=CARTESIAN_POINT('Ctrl Pts',(-88.7335807470613,184.165362726249,52.0991989146755));
#21203=CARTESIAN_POINT('Ctrl Pts',(-88.6694503783405,184.177428643762,52.169750856651));
#21204=CARTESIAN_POINT('Ctrl Pts',(-88.6048206625496,184.189556961584,52.2397358175433));
#21205=CARTESIAN_POINT('Ctrl Pts',(-88.4520875106276,184.218218641212,52.405124501888));
#21206=CARTESIAN_POINT('Ctrl Pts',(-88.2966148012104,184.24721896858,52.5672961007393));
#21207=CARTESIAN_POINT('Ctrl Pts',(-88.138680219344,184.276488112159,52.7265149727087));
#21208=CARTESIAN_POINT('Ctrl Pts',(-88.0074095306954,184.300815783708,52.8588531264069));
#21209=CARTESIAN_POINT('Ctrl Pts',(-87.8744370528921,184.325329410138,52.9891510658943));
#21210=CARTESIAN_POINT('Ctrl Pts',(-87.7398968895164,184.349994645736,53.1175521934523));
#21211=CARTESIAN_POINT('Ctrl Pts',(-87.5669079643352,184.381708689248,53.2826476749131));
#21212=CARTESIAN_POINT('Ctrl Pts',(-87.3913260249385,184.41367354028,53.4446068601911));
#21213=CARTESIAN_POINT('Ctrl Pts',(-87.2133483459065,184.445833478442,53.6037055710983));
#21214=CARTESIAN_POINT('Ctrl Pts',(-87.0353706668745,184.477993416603,53.7628042820054));
#21215=CARTESIAN_POINT('Ctrl Pts',(-86.8549969608648,184.510348541428,53.9190424247838));
#21216=CARTESIAN_POINT('Ctrl Pts',(-86.6723757709748,184.542853504445,54.0726796240347));
#21217=CARTESIAN_POINT('Ctrl Pts',(-86.475292839042,184.577932530146,54.2384833278686));
#21218=CARTESIAN_POINT('Ctrl Pts',(-86.2756058929237,184.613182555372,54.4012426705288));
#21219=CARTESIAN_POINT('Ctrl Pts',(-86.0735521960395,184.648540151242,54.5611869623873));
#21220=CARTESIAN_POINT('Ctrl Pts',(-85.8543878629899,184.686891955918,54.7346759140415));
#21221=CARTESIAN_POINT('Ctrl Pts',(-85.6324370091774,184.725370702841,54.9048521957901));
#21222=CARTESIAN_POINT('Ctrl Pts',(-85.4079128581921,184.763913428892,55.0719790830492));
#21223=CARTESIAN_POINT('Ctrl Pts',(-85.1783322433329,184.803324168032,55.2428698017895));
#21224=CARTESIAN_POINT('Ctrl Pts',(-84.9460610318809,184.842801868036,55.4105722034497));
#21225=CARTESIAN_POINT('Ctrl Pts',(-84.711276707351,184.882290320516,55.5753510661694));
#21226=CARTESIAN_POINT('Ctrl Pts',(-84.6589544714057,184.891090414526,55.6120724211887));
#21227=CARTESIAN_POINT('Ctrl Pts',(-84.6065072349179,184.899891083013,55.6486485206267));
#21228=CARTESIAN_POINT('Ctrl Pts',(-84.5539366380794,184.908691771476,55.6850821875323));
#21229=CARTESIAN_POINT('Ctrl Pts',(-84.4339755441047,184.928774104173,55.7682203446458));
#21230=CARTESIAN_POINT('Ctrl Pts',(-84.3133857020704,184.948853940928,55.8506069627194));
#21231=CARTESIAN_POINT('Ctrl Pts',(-84.1921856924569,184.968924862174,55.9322745501777));
#21232=CARTESIAN_POINT('Ctrl Pts',(-83.9861474492598,185.003045134655,56.0711082540669));
#21233=CARTESIAN_POINT('Ctrl Pts',(-83.7781170348905,185.037173395447,56.2079845765804));
#21234=CARTESIAN_POINT('Ctrl Pts',(-83.568516464438,185.071229092963,56.3428494397901));
#21235=CARTESIAN_POINT('Ctrl Pts',(-83.3489960646454,185.106896554735,56.4840970930091));
#21236=CARTESIAN_POINT('Ctrl Pts',(-83.1277532697727,185.142484462688,56.6231385182653));
#21237=CARTESIAN_POINT('Ctrl Pts',(-82.9052153450518,185.177909732773,56.7599207635829));
#21238=CARTESIAN_POINT('Ctrl Pts',(-82.7026785012987,185.210151079506,56.884409406509));
#21239=CARTESIAN_POINT('Ctrl Pts',(-82.4990678825317,185.242257885112,57.0070269383323));
#21240=CARTESIAN_POINT('Ctrl Pts',(-82.2946689193971,185.274173280065,57.1277380489338));
#21241=CARTESIAN_POINT('Ctrl Pts',(-82.2352099679613,185.283457358074,57.1628524935129));
#21242=CARTESIAN_POINT('Ctrl Pts',(-82.1756788543776,185.292726231422,57.1978089829018));
#21243=CARTESIAN_POINT('Ctrl Pts',(-82.1160839107254,185.301978283238,57.2326055443681));
#21244=CARTESIAN_POINT('Ctrl Pts',(-81.7887439000654,185.352797472826,57.4237342895821));
#21245=CARTESIAN_POINT('Ctrl Pts',(-81.4591756081384,185.403164059862,57.6102890632906));
#21246=CARTESIAN_POINT('Ctrl Pts',(-81.1276197694625,185.453012021079,57.7926461799151));
#21247=CARTESIAN_POINT('Ctrl Pts',(-80.7875849553267,185.504134758942,57.9796667689819));
#21248=CARTESIAN_POINT('Ctrl Pts',(-80.4454595429424,185.554712071923,58.1622722017703));
#21249=CARTESIAN_POINT('Ctrl Pts',(-80.1014577657148,185.604680843576,58.3408392875945));
#21250=CARTESIAN_POINT('Ctrl Pts',(-80.032898979013,185.614639508282,58.3764273093997));
#21251=CARTESIAN_POINT('Ctrl Pts',(-79.9642655255146,185.624574025262,58.4118548409497));
#21252=CARTESIAN_POINT('Ctrl Pts',(-79.8955588980838,185.634483928414,58.4471247348226));
#21253=CARTESIAN_POINT('Ctrl Pts',(-79.5316246154641,185.68697600421,58.6339469382209));
#21254=CARTESIAN_POINT('Ctrl Pts',(-79.1656381332745,185.738777667491,58.81634686547));
#21255=CARTESIAN_POINT('Ctrl Pts',(-78.797734523417,185.78983874123,58.9946950423225));
#21256=CARTESIAN_POINT('Ctrl Pts',(-78.4204446175163,185.842202532152,59.1775934022715));
#21257=CARTESIAN_POINT('Ctrl Pts',(-78.0411384098941,185.893787548864,59.3562305679962));
#21258=CARTESIAN_POINT('Ctrl Pts',(-77.6599161892546,185.944545250797,59.5309767423899));
#21259=CARTESIAN_POINT('Ctrl Pts',(-77.6239543810173,185.949333373432,59.5474610606523));
#21260=CARTESIAN_POINT('Ctrl Pts',(-77.5879754909047,185.95411413746,59.563910733478));
#21261=CARTESIAN_POINT('Ctrl Pts',(-77.5519795834612,185.958887504175,59.5803260588794));
#21262=CARTESIAN_POINT('Ctrl Pts',(-77.5509731104167,185.959020971152,59.5807850439059));
#21263=CARTESIAN_POINT('Ctrl Pts',(-77.5499666241808,185.959154432318,59.5812440021455));
#21264=CARTESIAN_POINT('Ctrl Pts',(-77.5489601247535,185.959287887672,59.581702933604));
#21265=CARTESIAN_POINT('Ctrl Pts',(-77.104093236163,186.018274377647,59.7845479670832));
#21266=CARTESIAN_POINT('Ctrl Pts',(-76.656675622457,186.076124505428,59.9821566691924));
#21267=CARTESIAN_POINT('Ctrl Pts',(-76.2069171712731,186.132768524725,60.1749241646176));
#21268=CARTESIAN_POINT('Ctrl Pts',(-75.7497127441504,186.190350314071,60.3708830222705));
#21269=CARTESIAN_POINT('Ctrl Pts',(-75.2900891958921,186.246685825175,60.5618389662368));
#21270=CARTESIAN_POINT('Ctrl Pts',(-74.8282214571534,186.301708554694,60.7481774544196));
#21271=CARTESIAN_POINT('Ctrl Pts',(-74.3542859546025,186.358168928042,60.9393846283233));
#21272=CARTESIAN_POINT('Ctrl Pts',(-73.8779873816825,186.413247119223,61.1257298593644));
#21273=CARTESIAN_POINT('Ctrl Pts',(-73.3994686781298,186.466876867152,61.3075995918588));
#21274=CARTESIAN_POINT('Ctrl Pts',(-73.1328670620181,186.49675611192,61.4089263827342));
#21275=CARTESIAN_POINT('Ctrl Pts',(-72.8655754995583,186.526185844042,61.5088634323636));
#21276=CARTESIAN_POINT('Ctrl Pts',(-72.597612901913,186.555155155028,61.607473776701));
#21277=CARTESIAN_POINT('Ctrl Pts',(-72.5779166749682,186.557284504902,61.6147219961848));
#21278=CARTESIAN_POINT('Ctrl Pts',(-72.5582170481678,186.559411341513,61.6219629615358));
#21279=CARTESIAN_POINT('Ctrl Pts',(-72.5385140095715,186.561535662791,61.6291967046453));
#21280=CARTESIAN_POINT('Ctrl Pts',(-72.1599131996972,186.602355242599,61.7681956202845));
#21281=CARTESIAN_POINT('Ctrl Pts',(-71.7796564183865,186.642285282424,61.9046445763352));
#21282=CARTESIAN_POINT('Ctrl Pts',(-71.3982081963154,186.681262919249,62.0385496296937));
#21283=CARTESIAN_POINT('Ctrl Pts',(-70.9933353519151,186.722634161206,62.1806777527151));
#21284=CARTESIAN_POINT('Ctrl Pts',(-70.5871199280422,186.762932566114,62.3199401712124));
#21285=CARTESIAN_POINT('Ctrl Pts',(-70.1800592229702,186.802083325186,62.4563372032453));
#21286=CARTESIAN_POINT('Ctrl Pts',(-70.0819837581538,186.811516141584,62.4892001206174));
#21287=CARTESIAN_POINT('Ctrl Pts',(-69.9838589874606,186.8208823333,62.5218966629664));
#21288=CARTESIAN_POINT('Ctrl Pts',(-69.8856914387029,186.830180842981,62.5544267552581));
#21289=CARTESIAN_POINT('Ctrl Pts',(-69.3917334939288,186.876968939349,62.7181111676227));
#21290=CARTESIAN_POINT('Ctrl Pts',(-68.8971169074742,186.922014017036,62.8774716062755));
#21291=CARTESIAN_POINT('Ctrl Pts',(-68.4014114556514,186.965338130696,63.032944115052));
#21292=CARTESIAN_POINT('Ctrl Pts',(-68.1010971848464,186.991585269101,63.1271343502648));
#21293=CARTESIAN_POINT('Ctrl Pts',(-67.8003826648161,187.017200505675,63.2198967397514));
#21294=CARTESIAN_POINT('Ctrl Pts',(-67.4991671307146,187.042186255654,63.3113209645549));
#21295=CARTESIAN_POINT('Ctrl Pts',(-67.3897881220146,187.051259215893,63.3445194219652));
#21296=CARTESIAN_POINT('Ctrl Pts',(-67.2803598516228,187.060247713469,63.3775362262536));
#21297=CARTESIAN_POINT('Ctrl Pts',(-67.1708834291509,187.0691513977,63.4103738904999));
#21298=CARTESIAN_POINT('Ctrl Pts',(-66.3906302403782,187.132609152859,63.6444123406198));
#21299=CARTESIAN_POINT('Ctrl Pts',(-65.6079560695515,187.191753398071,63.8693796059803));
#21300=CARTESIAN_POINT('Ctrl Pts',(-64.8230945608355,187.246495462802,64.0859928487631));
#21301=CARTESIAN_POINT('Ctrl Pts',(-64.0188735114315,187.302587805534,64.3079491142838));
#21302=CARTESIAN_POINT('Ctrl Pts',(-63.2123558151995,187.354058220625,64.5211340667888));
#21303=CARTESIAN_POINT('Ctrl Pts',(-62.4037608425511,187.400808838323,64.7262749266695));
#21304=CARTESIAN_POINT('Ctrl Pts',(-62.1386954729806,187.416134149729,64.7935221142945));
#21305=CARTESIAN_POINT('Ctrl Pts',(-61.8734066350219,187.430952249136,64.8599045480167));
#21306=CARTESIAN_POINT('Ctrl Pts',(-61.6079013555631,187.445259604425,64.9254468698671));
#21307=CARTESIAN_POINT('Ctrl Pts',(-60.7321298652538,187.492452541188,65.1416387926877));
#21308=CARTESIAN_POINT('Ctrl Pts',(-59.8539948749924,187.534092962162,65.3486811914531));
#21309=CARTESIAN_POINT('Ctrl Pts',(-58.9735550061956,187.570087849531,65.5472366543624));
#21310=CARTESIAN_POINT('Ctrl Pts',(-58.3473067264981,187.595690661366,65.6884672159015));
#21311=CARTESIAN_POINT('Ctrl Pts',(-57.7198916747325,187.618437051291,65.8254029884363));
#21312=CARTESIAN_POINT('Ctrl Pts',(-57.0913221019793,187.638290733231,65.9582694164764));
#21313=CARTESIAN_POINT('Ctrl Pts',(-56.6910661901281,187.65093301487,66.0428751238075));
#21314=CARTESIAN_POINT('Ctrl Pts',(-56.2903567688877,187.662400400639,66.1258265383601));
#21315=CARTESIAN_POINT('Ctrl Pts',(-55.8892136405948,187.67268314244,66.2071768544313));
#21316=CARTESIAN_POINT('Ctrl Pts',(-54.8268757205327,187.699914685915,66.4226149848045));
#21317=CARTESIAN_POINT('Ctrl Pts',(-53.7614897889712,187.718841660279,66.6268177710292));
#21318=CARTESIAN_POINT('Ctrl Pts',(-52.6932101568605,187.729309460939,66.8205301740338));
#21319=CARTESIAN_POINT('Ctrl Pts',(-52.3976784406378,187.73220530113,66.8741192879631));
#21320=CARTESIAN_POINT('Ctrl Pts',(-52.1019250975687,187.734453729065,66.9269053030203));
#21321=CARTESIAN_POINT('Ctrl Pts',(-51.8059530143082,187.73605141499,66.9789034094812));
#21322=CARTESIAN_POINT('Ctrl Pts',(-51.2156484509358,187.739237936104,67.0826115673333));
#21323=CARTESIAN_POINT('Ctrl Pts',(-50.6246907854393,187.739834061284,67.183148451155));
#21324=CARTESIAN_POINT('Ctrl Pts',(-50.0325609317261,187.737811001709,67.2807215961937));
#21325=CARTESIAN_POINT('Ctrl Pts',(-49.3669370627525,187.735536843882,67.3904053317819));
#21326=CARTESIAN_POINT('Ctrl Pts',(-48.7005037624025,187.729943847346,67.4962109139689));
#21327=CARTESIAN_POINT('Ctrl Pts',(-48.0342097043618,187.721039705149,67.5981665837054));
#21328=CARTESIAN_POINT('Ctrl Pts',(-47.7114780816944,187.716726822233,67.6475506632078));
#21329=CARTESIAN_POINT('Ctrl Pts',(-47.3887787089,187.711636603788,67.6960309549637));
#21330=CARTESIAN_POINT('Ctrl Pts',(-47.0662186498782,187.705767111222,67.7436074595605));
#21331=CARTESIAN_POINT('Ctrl Pts',(-46.8709828487003,187.702214485745,67.7724040719506));
#21332=CARTESIAN_POINT('Ctrl Pts',(-46.6757335248632,187.698376276571,67.8008803204517));
#21333=CARTESIAN_POINT('Ctrl Pts',(-46.4804497524561,187.694251645111,67.8290426111402));
#21334=CARTESIAN_POINT('Ctrl Pts',(-45.6873485229294,187.677500379801,67.9434174365343));
#21335=CARTESIAN_POINT('Ctrl Pts',(-44.8942928337594,187.656037737837,68.0525249655041));
#21336=CARTESIAN_POINT('Ctrl Pts',(-44.1013097658917,187.629850768109,68.156604155172));
#21337=CARTESIAN_POINT('Ctrl Pts',(-42.1265420022274,187.564637290365,68.4157928276074));
#21338=CARTESIAN_POINT('Ctrl Pts',(-40.1522371157117,187.470128839998,68.6438522044417));
#21339=CARTESIAN_POINT('Ctrl Pts',(-38.1786286591264,187.346091518818,68.8436843142897));
#21340=CARTESIAN_POINT('Ctrl Pts',(-37.3942034702417,187.296791973728,68.9231090552963));
#21341=CARTESIAN_POINT('Ctrl Pts',(-36.6098926799408,187.242833017126,68.9980981274691));
#21342=CARTESIAN_POINT('Ctrl Pts',(-35.8256957544281,187.18419137613,69.0687626934297));
#21343=CARTESIAN_POINT('Ctrl Pts',(-34.0772988235321,187.053447602716,69.2263120362401));
#21344=CARTESIAN_POINT('Ctrl Pts',(-32.3294901451123,186.899468346254,69.3623707313213));
#21345=CARTESIAN_POINT('Ctrl Pts',(-30.5823941605077,186.722004943281,69.4781726760757));
#21346=CARTESIAN_POINT('Ctrl Pts',(-29.1744261304627,186.578988875422,69.571496361476));
#21347=CARTESIAN_POINT('Ctrl Pts',(-27.7669210639304,186.420721359934,69.6516650119064));
#21348=CARTESIAN_POINT('Ctrl Pts',(-26.3599459146534,186.247088364698,69.7193429471197));
#21349=CARTESIAN_POINT('Ctrl Pts',(-25.9684093601055,186.198769341619,69.7381765317683));
#21350=CARTESIAN_POINT('Ctrl Pts',(-25.5769128675606,186.149260825002,69.7560409460401));
#21351=CARTESIAN_POINT('Ctrl Pts',(-25.185456477602,186.098558361674,69.7729424130737));
#21352=CARTESIAN_POINT('Ctrl Pts',(-23.4136314921367,185.869066919834,69.849442483961));
#21353=CARTESIAN_POINT('Ctrl Pts',(-21.6426480519369,185.615155774587,69.9062160012814));
#21354=CARTESIAN_POINT('Ctrl Pts',(-19.8725824218587,185.336465133903,69.9438553294453));
#21355=CARTESIAN_POINT('Ctrl Pts',(-18.1025167917806,185.057774493219,69.9814946576092));
#21356=CARTESIAN_POINT('Ctrl Pts',(-16.3333689159223,184.754304176831,70.));
#21357=CARTESIAN_POINT('Ctrl Pts',(-14.5652173913043,184.425742352699,70.));
#21358=CARTESIAN_POINT('Origin',(3.92135447228743,250.,-28.0096748020595));
#21359=CARTESIAN_POINT('Origin',(-126.751426934183,250.,-46.3038641989654));
#21360=CARTESIAN_POINT('Origin',(-108.033967922038,250.,-180.));
#21361=CARTESIAN_POINT('Origin',(-115.000000000001,250.,-45.1798442476466));
#21362=CARTESIAN_POINT('Ctrl Pts',(-108.033967922038,249.902929948988,-69.9999999999999));
#21363=CARTESIAN_POINT('Ctrl Pts',(-107.337364714242,274.893222943887,-69.9999999999999));
#21364=CARTESIAN_POINT('Ctrl Pts',(-107.337364714242,274.893222943887,-44.9999999999999));
#21365=CARTESIAN_POINT('Ctrl Pts',(-109.926868419224,249.967686392606,-69.9999999999999));
#21366=CARTESIAN_POINT('Ctrl Pts',(-109.462400534848,274.952458214507,-69.988015594096));
#21367=CARTESIAN_POINT('Ctrl Pts',(-109.892780719038,274.964455041348,-44.9999999999515));
#21368=CARTESIAN_POINT('Ctrl Pts',(-111.81888094899,250.000000000097,-70.0488277014676));
#21369=CARTESIAN_POINT('Ctrl Pts',(-111.587915676122,274.988026907036,-70.0368939405427));
#21370=CARTESIAN_POINT('Ctrl Pts',(-112.446996903964,275.,-45.0599248876671));
#21371=CARTESIAN_POINT('Ctrl Pts',(-113.709994059637,250.,-70.1465397573417));
#21372=CARTESIAN_POINT('Ctrl Pts',(-113.709994059638,275.,-70.1465397573417));
#21373=CARTESIAN_POINT('Ctrl Pts',(-115.000000000001,275.,-45.1798442476466));
#21374=CARTESIAN_POINT('Origin',(-108.033967922038,249.902929948988,-44.9999999999999));
#21375=CARTESIAN_POINT('Origin',(-115.,0.,-44.9999999999999));
#21376=CARTESIAN_POINT('Ctrl Pts',(160.,1.95943487863576E-14,-45.));
#21377=CARTESIAN_POINT('Ctrl Pts',(160.,0.241428813471072,-45.0423872342559));
#21378=CARTESIAN_POINT('Ctrl Pts',(159.999569933784,0.485776692267064,-45.0852869669719));
#21379=CARTESIAN_POINT('Ctrl Pts',(159.998704815839,0.729365769049337,-45.1280532951593));
#21380=CARTESIAN_POINT('Ctrl Pts',(159.998619971277,0.753255238303078,-45.1322475098417));
#21381=CARTESIAN_POINT('Ctrl Pts',(159.998530983713,0.777137409236483,-45.1364404414182));
#21382=CARTESIAN_POINT('Ctrl Pts',(159.99843787551,0.801008812615739,-45.1406314806358));
#21383=CARTESIAN_POINT('Ctrl Pts',(159.997395389115,1.06828508400977,-45.1875564694));
#21384=CARTESIAN_POINT('Ctrl Pts',(159.995831384815,1.33549350879009,-45.2344693061509));
#21385=CARTESIAN_POINT('Ctrl Pts',(159.993746619827,1.60263422617359,-45.2813697753231));
#21386=CARTESIAN_POINT('Ctrl Pts',(159.989577089851,2.13691566094059,-45.3751707136674));
#21387=CARTESIAN_POINT('Ctrl Pts',(159.983324543108,2.67092626652068,-45.4689221824702));
#21388=CARTESIAN_POINT('Ctrl Pts',(159.974994723865,3.20466712940897,-45.5626224552081));
#21389=CARTESIAN_POINT('Ctrl Pts',(159.958335085379,4.27214885518554,-45.750023000684));
#21390=CARTESIAN_POINT('Ctrl Pts',(159.933366764185,5.33855161416616,-45.9372187695708));
#21391=CARTESIAN_POINT('Ctrl Pts',(159.900130777316,6.40388332360616,-46.1241959387466));
#21392=CARTESIAN_POINT('Ctrl Pts',(159.844073645198,8.20071398858914,-46.4395590395064));
#21393=CARTESIAN_POINT('Ctrl Pts',(159.764499768404,9.9944985583727,-46.7543004148088));
#21394=CARTESIAN_POINT('Ctrl Pts',(159.66156459619,11.7852683761882,-47.0683529511729));
#21395=CARTESIAN_POINT('Ctrl Pts',(159.642440294338,12.117975086691,-47.1267006993085));
#21396=CARTESIAN_POINT('Ctrl Pts',(159.622509467296,12.4505777513804,-47.1850246736135));
#21397=CARTESIAN_POINT('Ctrl Pts',(159.601772915272,12.7830765913653,-47.2433244470768));
#21398=CARTESIAN_POINT('Ctrl Pts',(159.488946002297,14.5921920913896,-47.5605316404166));
#21399=CARTESIAN_POINT('Ctrl Pts',(159.352270449035,16.3982349599817,-47.8770224280089));
#21400=CARTESIAN_POINT('Ctrl Pts',(159.191844897926,18.201227162187,-48.1927256439253));
#21401=CARTESIAN_POINT('Ctrl Pts',(159.031054793873,20.0083165054632,-48.5091462676101));
#21402=CARTESIAN_POINT('Ctrl Pts',(158.846406606695,21.8123416173502,-48.8247758695827));
#21403=CARTESIAN_POINT('Ctrl Pts',(158.63794737614,23.6133234274148,-49.1395408988029));
#21404=CARTESIAN_POINT('Ctrl Pts',(158.56644346243,24.2310809025642,-49.2475089241488));
#21405=CARTESIAN_POINT('Ctrl Pts',(158.492137565761,24.8484802804144,-49.3553752009994));
#21406=CARTESIAN_POINT('Ctrl Pts',(158.415030182465,25.4655222709345,-49.4631366661702));
#21407=CARTESIAN_POINT('Ctrl Pts',(158.192546930629,27.2459160892981,-49.7740682549364));
#21408=CARTESIAN_POINT('Ctrl Pts',(157.946747091716,29.0233150502689,-50.0841213897866));
#21409=CARTESIAN_POINT('Ctrl Pts',(157.67760762034,30.7977467655214,-50.393226320715));
#21410=CARTESIAN_POINT('Ctrl Pts',(157.408614074615,32.5712163955664,-50.7021636569825));
#21411=CARTESIAN_POINT('Ctrl Pts',(157.116306108476,34.3417222960772,-51.0101539483635));
#21412=CARTESIAN_POINT('Ctrl Pts',(156.800610504028,36.1092800826396,-51.3171210658553));
#21413=CARTESIAN_POINT('Ctrl Pts',(156.48528503735,37.8747654935152,-51.6237282793055));
#21414=CARTESIAN_POINT('Ctrl Pts',(156.146626628634,39.6373099897026,-51.9293148460777));
#21415=CARTESIAN_POINT('Ctrl Pts',(155.784513744485,41.3969127896342,-52.2337964757992));
#21416=CARTESIAN_POINT('Ctrl Pts',(155.423406849553,43.1516272204391,-52.5374322222349));
#21417=CARTESIAN_POINT('Ctrl Pts',(155.038975473555,44.9034165515896,-52.8399692873509));
#21418=CARTESIAN_POINT('Ctrl Pts',(154.631052697224,46.6522595283741,-53.1413137955519));
#21419=CARTESIAN_POINT('Ctrl Pts',(154.329106510401,47.9467605928748,-53.3643702916616));
#21420=CARTESIAN_POINT('Ctrl Pts',(154.01428836003,49.2396469405541,-53.5867731807701));
#21421=CARTESIAN_POINT('Ctrl Pts',(153.686514832082,50.5309013666428,-53.8084801340299));
#21422=CARTESIAN_POINT('Ctrl Pts',(153.459876360839,51.4237371332936,-53.9617790452175));
#21423=CARTESIAN_POINT('Ctrl Pts',(153.226916829294,52.3162715954779,-54.1148283740067));
#21424=CARTESIAN_POINT('Ctrl Pts',(152.987866013332,53.2074993271734,-54.267442333427));
#21425=CARTESIAN_POINT('Ctrl Pts',(152.748770608958,54.0988932931027,-54.4200847588203));
#21426=CARTESIAN_POINT('Ctrl Pts',(152.503581686487,54.9889799168632,-54.5722916107141));
#21427=CARTESIAN_POINT('Ctrl Pts',(152.252579004115,55.8767679003207,-54.7238815612453));
#21428=CARTESIAN_POINT('Ctrl Pts',(152.172094921845,56.1614373724718,-54.772488922468));
#21429=CARTESIAN_POINT('Ctrl Pts',(152.091013469055,56.4458706268006,-54.8210328936362));
#21430=CARTESIAN_POINT('Ctrl Pts',(152.009344941798,56.7300353333953,-54.8695076066916));
#21431=CARTESIAN_POINT('Ctrl Pts',(151.512006252958,58.4605196134401,-55.1647051698487));
#21432=CARTESIAN_POINT('Ctrl Pts',(150.992598450078,60.1821039252991,-55.4575143567747));
#21433=CARTESIAN_POINT('Ctrl Pts',(150.451275564066,61.8948642781311,-55.7478609014618));
#21434=CARTESIAN_POINT('Ctrl Pts',(150.349315513962,62.2174686532709,-55.8025486839458));
#21435=CARTESIAN_POINT('Ctrl Pts',(150.246577836907,62.5397599556456,-55.8571490762826));
#21436=CARTESIAN_POINT('Ctrl Pts',(150.143063362087,62.8617386556575,-55.9116615490075));
#21437=CARTESIAN_POINT('Ctrl Pts',(149.588997306711,64.5851446676367,-56.2034421022505));
#21438=CARTESIAN_POINT('Ctrl Pts',(149.01268050901,66.2995961835638,-56.4927037319273));
#21439=CARTESIAN_POINT('Ctrl Pts',(148.414211986665,68.0051470032801,-56.7793615666974));
#21440=CARTESIAN_POINT('Ctrl Pts',(147.813151839321,69.7180835884611,-57.0672607526555));
#21441=CARTESIAN_POINT('Ctrl Pts',(147.189747552607,71.4220425040294,-57.3525336847906));
#21442=CARTESIAN_POINT('Ctrl Pts',(146.544050740992,73.1170624313016,-57.635082586302));
#21443=CARTESIAN_POINT('Ctrl Pts',(146.3170290416,73.7130175258135,-57.7344244610465));
#21444=CARTESIAN_POINT('Ctrl Pts',(146.087251184375,74.3078674490983,-57.8334294837149));
#21445=CARTESIAN_POINT('Ctrl Pts',(145.854718046044,74.9016133224768,-57.9320930104149));
#21446=CARTESIAN_POINT('Ctrl Pts',(145.206033961624,76.5579514298781,-58.207328875473));
#21447=CARTESIAN_POINT('Ctrl Pts',(144.535923549658,78.2056781948319,-58.4798984641246));
#21448=CARTESIAN_POINT('Ctrl Pts',(143.844362799228,79.8448249563277,-58.7497069691199));
#21449=CARTESIAN_POINT('Ctrl Pts',(143.1513853196,81.4873296687725,-59.020068202978));
#21450=CARTESIAN_POINT('Ctrl Pts',(142.436869320226,83.1212194287967,-59.2876571684577));
#21451=CARTESIAN_POINT('Ctrl Pts',(141.700748012094,84.7465005374518,-59.5523615928747));
#21452=CARTESIAN_POINT('Ctrl Pts',(140.964375086706,86.372337191461,-59.8171564972169));
#21453=CARTESIAN_POINT('Ctrl Pts',(140.206381845747,87.9895595256459,-60.0790650220006));
#21454=CARTESIAN_POINT('Ctrl Pts',(139.426662132564,89.5981451905916,-60.3379558580429));
#21455=CARTESIAN_POINT('Ctrl Pts',(138.647119944871,91.2063646150111,-60.5967877501831));
#21456=CARTESIAN_POINT('Ctrl Pts',(137.845860923211,92.8059514987935,-60.8526034576932));
#21457=CARTESIAN_POINT('Ctrl Pts',(137.022743375541,94.3968517670101,-61.1052508746052));
#21458=CARTESIAN_POINT('Ctrl Pts',(136.382274663422,95.6347330985131,-61.301836120768));
#21459=CARTESIAN_POINT('Ctrl Pts',(135.728571144476,96.8673545851268,-61.4965027555554));
#21460=CARTESIAN_POINT('Ctrl Pts',(135.061552680395,98.0946763544619,-61.6891696133877));
#21461=CARTESIAN_POINT('Ctrl Pts',(134.239401643232,99.6074438713001,-61.9266461834137));
#21462=CARTESIAN_POINT('Ctrl Pts',(133.397005184789,101.112182410997,-62.1610953092384));
#21463=CARTESIAN_POINT('Ctrl Pts',(132.534149953513,102.608830985837,-62.3923631872123));
#21464=CARTESIAN_POINT('Ctrl Pts',(132.322774384846,102.975468322129,-62.4490173946031));
#21465=CARTESIAN_POINT('Ctrl Pts',(132.110170926118,103.34161999574,-62.5054805761156));
#21466=CARTESIAN_POINT('Ctrl Pts',(131.896336194158,103.707284769956,-62.5617502437278));
#21467=CARTESIAN_POINT('Ctrl Pts',(131.150525617363,104.982646605105,-62.7580070111533));
#21468=CARTESIAN_POINT('Ctrl Pts',(130.391368173285,106.249286509145,-62.9514793059366));
#21469=CARTESIAN_POINT('Ctrl Pts',(129.619361911524,107.506510787503,-63.141982854025));
#21470=CARTESIAN_POINT('Ctrl Pts',(129.266469660511,108.081201340666,-63.2290640465498));
#21471=CARTESIAN_POINT('Ctrl Pts',(128.910893216072,108.653924930634,-63.3155250005697));
#21472=CARTESIAN_POINT('Ctrl Pts',(128.552682965157,109.224617543254,-63.4013485459176));
#21473=CARTESIAN_POINT('Ctrl Pts',(127.593775576704,110.752327488401,-63.6310930368334));
#21474=CARTESIAN_POINT('Ctrl Pts',(126.615676477573,112.266004480819,-63.8563473482364));
#21475=CARTESIAN_POINT('Ctrl Pts',(125.618464049675,113.765729384398,-64.0769716167984));
#21476=CARTESIAN_POINT('Ctrl Pts',(124.614206339913,115.276049808418,-64.2991545905214));
#21477=CARTESIAN_POINT('Ctrl Pts',(123.590563995459,116.77222047651,-64.5166420286909));
#21478=CARTESIAN_POINT('Ctrl Pts',(122.547579997488,118.254296304307,-64.7292655492744));
#21479=CARTESIAN_POINT('Ctrl Pts',(122.15972197473,118.805440906012,-64.8083345843179));
#21480=CARTESIAN_POINT('Ctrl Pts',(121.769188853402,119.354636048327,-64.8867307245452));
#21481=CARTESIAN_POINT('Ctrl Pts',(121.375981673587,119.901883520301,-64.9644443511221));
#21482=CARTESIAN_POINT('Ctrl Pts',(120.35986499798,121.31606746836,-65.1652700632155));
#21483=CARTESIAN_POINT('Ctrl Pts',(119.32592306836,122.717230533083,-65.3615257399208));
#21484=CARTESIAN_POINT('Ctrl Pts',(118.274111846381,124.105401649993,-65.553052721444));
#21485=CARTESIAN_POINT('Ctrl Pts',(117.217260755787,125.500224340776,-65.7454974254661));
#21486=CARTESIAN_POINT('Ctrl Pts',(116.142368392054,126.881930373277,-65.9331681660453));
#21487=CARTESIAN_POINT('Ctrl Pts',(115.049363967163,128.250516040694,-66.1158723525937));
#21488=CARTESIAN_POINT('Ctrl Pts',(113.954288243496,129.621695247307,-66.2989227728345));
#21489=CARTESIAN_POINT('Ctrl Pts',(112.841031394603,130.97970435778,-66.4769879351814));
#21490=CARTESIAN_POINT('Ctrl Pts',(111.709501198964,132.324505533451,-66.6498402760476));
#21491=CARTESIAN_POINT('Ctrl Pts',(110.575125429341,133.672688617315,-66.8231273062629));
#21492=CARTESIAN_POINT('Ctrl Pts',(109.422383925239,135.007597262524,-66.9911753997619));
#21493=CARTESIAN_POINT('Ctrl Pts',(108.251168041227,136.329158679192,-67.1537191905785));
#21494=CARTESIAN_POINT('Ctrl Pts',(107.205533034561,137.509018771246,-67.2988346044949));
#21495=CARTESIAN_POINT('Ctrl Pts',(106.145172602991,138.678239943829,-67.4395623725332));
#21496=CARTESIAN_POINT('Ctrl Pts',(105.070002502002,139.836747253322,-67.575688188434));
#21497=CARTESIAN_POINT('Ctrl Pts',(104.335872795981,140.62777988133,-67.6686353463928));
#21498=CARTESIAN_POINT('Ctrl Pts',(103.594385160809,141.414284085743,-67.759495179416));
#21499=CARTESIAN_POINT('Ctrl Pts',(102.846253577245,142.195425520933,-67.8481017411357));
#21500=CARTESIAN_POINT('Ctrl Pts',(102.098121993682,142.976566956123,-67.9367083028554));
#21501=CARTESIAN_POINT('Ctrl Pts',(101.343346621331,143.752345521681,-68.0230615341653));
#21502=CARTESIAN_POINT('Ctrl Pts',(100.58268168766,144.521972689812,-68.1070104348258));
#21503=CARTESIAN_POINT('Ctrl Pts',(99.325773062813,145.793690344617,-68.2457260408908));
#21504=CARTESIAN_POINT('Ctrl Pts',(98.0538833836472,147.047528667054,-68.3777624601209));
#21505=CARTESIAN_POINT('Ctrl Pts',(96.7671060577393,148.283619243825,-68.5028706402217));
#21506=CARTESIAN_POINT('Ctrl Pts',(96.4964012088721,148.543660904517,-68.5291901830861));
#21507=CARTESIAN_POINT('Ctrl Pts',(96.2250374009896,148.802917009055,-68.5552029557569));
#21508=CARTESIAN_POINT('Ctrl Pts',(95.9530153961869,149.061388643233,-68.5809064063632));
#21509=CARTESIAN_POINT('Ctrl Pts',(94.6909245240803,150.260610340133,-68.7001617968061));
#21510=CARTESIAN_POINT('Ctrl Pts',(93.4146742779891,151.4429502265,-68.8127591153259));
#21511=CARTESIAN_POINT('Ctrl Pts',(92.1243034092432,152.608485238147,-68.9184302559128));
#21512=CARTESIAN_POINT('Ctrl Pts',(90.8270487660792,153.780238059178,-69.0246651230313));
#21513=CARTESIAN_POINT('Ctrl Pts',(89.5155220275952,154.935006065013,-69.1238998529433));
#21514=CARTESIAN_POINT('Ctrl Pts',(88.189753472043,156.072844050722,-69.2158157195382));
#21515=CARTESIAN_POINT('Ctrl Pts',(87.5636550889273,156.610191629314,-69.2592232775292));
#21516=CARTESIAN_POINT('Ctrl Pts',(86.9343803601109,157.143763101884,-69.300997880872));
#21517=CARTESIAN_POINT('Ctrl Pts',(86.3019321777129,157.673562624529,-69.3411022734024));
#21518=CARTESIAN_POINT('Ctrl Pts',(85.0908680290335,158.688066619829,-69.41789748501));
#21519=CARTESIAN_POINT('Ctrl Pts',(83.8682332813244,159.688756437948,-69.4885573011914));
#21520=CARTESIAN_POINT('Ctrl Pts',(82.6339523845695,160.675622844142,-69.5528173901377));
#21521=CARTESIAN_POINT('Ctrl Pts',(81.4013292413063,161.661163797406,-69.6169911718366));
#21522=CARTESIAN_POINT('Ctrl Pts',(80.1570908588353,162.63291819202,-69.6747824784201));
#21523=CARTESIAN_POINT('Ctrl Pts',(78.9011663895971,163.590858124471,-69.7258797875447));
#21524=CARTESIAN_POINT('Ctrl Pts',(77.650965694506,164.54443232319,-69.7767442248173));
#21525=CARTESIAN_POINT('Ctrl Pts',(76.3891848535843,165.484317383387,-69.8209755698939));
#21526=CARTESIAN_POINT('Ctrl Pts',(75.1157634657088,166.410471429902,-69.858217964424));
#21527=CARTESIAN_POINT('Ctrl Pts',(73.8478440584874,167.332623908912,-69.8952994484054));
#21528=CARTESIAN_POINT('Ctrl Pts',(72.5683841627989,168.241163423421,-69.9254522553877));
#21529=CARTESIAN_POINT('Ctrl Pts',(71.2773384017722,169.136039253356,-69.9482765461247));
#21530=CARTESIAN_POINT('Ctrl Pts',(69.9972799515188,170.023299335543,-69.9709065931075));
#21531=CARTESIAN_POINT('Ctrl Pts',(68.7058317241478,170.897126922303,-69.9863322828695));
#21532=CARTESIAN_POINT('Ctrl Pts',(67.4029678704178,171.757468812413,-69.9941163663231));
#21533=CARTESIAN_POINT('Ctrl Pts',(66.7497755452623,172.18880223073,-69.9980189257162));
#21534=CARTESIAN_POINT('Ctrl Pts',(66.0937141832166,172.616745954954,-70.));
#21535=CARTESIAN_POINT('Ctrl Pts',(65.4347826086956,173.041293409847,-70.));
#21536=CARTESIAN_POINT('Origin',(3.92135447228745,250.,28.0096748020596));
#21537=CARTESIAN_POINT('Origin',(-126.751426934183,250.,46.3038641989655));
#21538=CARTESIAN_POINT('Origin',(-108.033967922038,250.,180.));
#21539=CARTESIAN_POINT('Origin',(-115.000000000001,250.,45.1798442476468));
#21540=CARTESIAN_POINT('Ctrl Pts',(-113.709994059637,250.,70.1465397573418));
#21541=CARTESIAN_POINT('Ctrl Pts',(-113.709994059638,275.,70.1465397573418));
#21542=CARTESIAN_POINT('Ctrl Pts',(-115.000000000001,275.,45.1798442476468));
#21543=CARTESIAN_POINT('Ctrl Pts',(-111.818880948996,250.000000000097,70.048827701468));
#21544=CARTESIAN_POINT('Ctrl Pts',(-111.587915676106,274.988026907036,70.0368939406218));
#21545=CARTESIAN_POINT('Ctrl Pts',(-112.446996903957,275.,45.0599248877022));
#21546=CARTESIAN_POINT('Ctrl Pts',(-109.926868419216,249.967686392701,70.0000000000001));
#21547=CARTESIAN_POINT('Ctrl Pts',(-109.462400534861,274.952458214506,69.9880155941608));
#21548=CARTESIAN_POINT('Ctrl Pts',(-109.892780719043,274.964455041348,44.9999999999839));
#21549=CARTESIAN_POINT('Ctrl Pts',(-108.033967922038,249.902929948988,70.0000000000001));
#21550=CARTESIAN_POINT('Ctrl Pts',(-107.337364714242,274.893222943887,70.));
#21551=CARTESIAN_POINT('Ctrl Pts',(-107.337364714242,274.893222943887,45.0000000000001));
#21552=CARTESIAN_POINT('Origin',(-108.033967922038,249.902929948988,45.0000000000001));
#21553=CARTESIAN_POINT('Origin',(-115.,0.,45.0000000000001));
#21554=CARTESIAN_POINT('Ctrl Pts',(65.4347826086958,173.041293409847,70.));
#21555=CARTESIAN_POINT('Ctrl Pts',(66.7484164009789,172.194923460766,70.));
#21556=CARTESIAN_POINT('Ctrl Pts',(68.0506414965792,171.335055332599,69.9921294361605));
#21557=CARTESIAN_POINT('Ctrl Pts',(69.341472894354,170.461741779368,69.9768486490774));
#21558=CARTESIAN_POINT('Ctrl Pts',(70.6413050269686,169.582338768026,69.9614613118182));
#21559=CARTESIAN_POINT('Ctrl Pts',(71.9295842856713,168.689302588284,69.938560099864));
#21560=CARTESIAN_POINT('Ctrl Pts',(73.2063469470379,167.78268628942,69.908566552343));
#21561=CARTESIAN_POINT('Ctrl Pts',(74.4928427896132,166.86915855667,69.8783443541557));
#21562=CARTESIAN_POINT('Ctrl Pts',(75.7676460752356,165.941843244657,69.8409213017712));
#21563=CARTESIAN_POINT('Ctrl Pts',(77.0308108162073,165.000787772658,69.7966789898779));
#21564=CARTESIAN_POINT('Ctrl Pts',(78.2972938165541,164.057260203362,69.752320456037));
#21565=CARTESIAN_POINT('Ctrl Pts',(79.5520773777388,163.099920519143,69.7011067518214));
#21566=CARTESIAN_POINT('Ctrl Pts',(80.7952280690075,162.128804309335,69.6433728837564));
#21567=CARTESIAN_POINT('Ctrl Pts',(82.0410026914299,161.155638354395,69.5855171562128));
#21568=CARTESIAN_POINT('Ctrl Pts',(83.2750956333978,160.168637936665,69.5211136521883));
#21569=CARTESIAN_POINT('Ctrl Pts',(84.4975809196787,159.167822048422,69.4504504842125));
#21570=CARTESIAN_POINT('Ctrl Pts',(85.1018573206763,158.673117179746,69.4155215690699));
#21571=CARTESIAN_POINT('Ctrl Pts',(85.7032976515598,158.175036435941,69.3790624569837));
#21572=CARTESIAN_POINT('Ctrl Pts',(86.301911080951,157.673580297207,69.3411036111759));
#21573=CARTESIAN_POINT('Ctrl Pts',(87.6416535312517,156.551283263696,69.2561488230001));
#21574=CARTESIAN_POINT('Ctrl Pts',(88.9671556757048,155.412061378825,69.1637022638884));
#21575=CARTESIAN_POINT('Ctrl Pts',(90.2783893218386,154.255869801442,69.0641054510097));
#21576=CARTESIAN_POINT('Ctrl Pts',(91.5830443271285,153.105478997367,68.965008329138));
#21577=CARTESIAN_POINT('Ctrl Pts',(92.8735740567254,151.938288542509,68.8588323958833));
#21578=CARTESIAN_POINT('Ctrl Pts',(94.1499446972401,150.75423258277,68.7458677221814));
#21579=CARTESIAN_POINT('Ctrl Pts',(94.7541325596118,150.193743163368,68.6923943167606));
#21580=CARTESIAN_POINT('Ctrl Pts',(95.3551476204497,149.629474299346,68.6373990733229));
#21581=CARTESIAN_POINT('Ctrl Pts',(95.9529854143453,149.061417131568,68.580909239356));
#21582=CARTESIAN_POINT('Ctrl Pts',(97.2460239280367,147.832789896195,68.4587297256198));
#21583=CARTESIAN_POINT('Ctrl Pts',(98.5241919067625,146.586439424219,68.3295643380909));
#21584=CARTESIAN_POINT('Ctrl Pts',(99.7874001697264,145.322239383386,68.1936707789836));
#21585=CARTESIAN_POINT('Ctrl Pts',(100.053145131183,145.056285778606,68.1650824379429));
#21586=CARTESIAN_POINT('Ctrl Pts',(100.318227953058,144.789542120827,68.1361961843661));
#21587=CARTESIAN_POINT('Ctrl Pts',(100.582647686213,144.52200709186,68.1070141873093));
#21588=CARTESIAN_POINT('Ctrl Pts',(101.343311973865,143.752380938002,68.0230654489202));
#21589=CARTESIAN_POINT('Ctrl Pts',(102.098086743775,142.97660336885,67.9367123807548));
#21590=CARTESIAN_POINT('Ctrl Pts',(102.84621774979,142.195462929158,67.8481059844437));
#21591=CARTESIAN_POINT('Ctrl Pts',(103.594348755805,141.414322489467,67.7594995881325));
#21592=CARTESIAN_POINT('Ctrl Pts',(104.335835838317,140.627819279647,67.6686399227833));
#21593=CARTESIAN_POINT('Ctrl Pts',(105.069964998763,139.836787663453,67.5756929366653));
#21594=CARTESIAN_POINT('Ctrl Pts',(106.274691395938,138.538682751708,67.4231643439496));
#21595=CARTESIAN_POINT('Ctrl Pts',(107.460824156216,137.227126993047,67.2648585766541));
#21596=CARTESIAN_POINT('Ctrl Pts',(108.628481350401,135.902223981139,67.1010750526694));
#21597=CARTESIAN_POINT('Ctrl Pts',(109.79344823223,134.580373580015,66.9376688901572));
#21598=CARTESIAN_POINT('Ctrl Pts',(110.940024958247,133.245237386367,66.7688100565757));
#21599=CARTESIAN_POINT('Ctrl Pts',(112.068318136567,131.896884093635,66.5947584549084));
#21600=CARTESIAN_POINT('Ctrl Pts',(113.194372744947,130.551205977185,66.4210521772144));
#21601=CARTESIAN_POINT('Ctrl Pts',(114.302216644142,129.192363144643,66.2421735841328));
#21602=CARTESIAN_POINT('Ctrl Pts',(115.391939711775,127.820389677704,66.0583456279631));
#21603=CARTESIAN_POINT('Ctrl Pts',(116.477450936578,126.453718967751,65.8752281775008));
#21604=CARTESIAN_POINT('Ctrl Pts',(117.544981473468,125.07401887109,65.6871994023175));
#21605=CARTESIAN_POINT('Ctrl Pts',(118.594598963408,123.681289636736,65.4944466132403));
#21606=CARTESIAN_POINT('Ctrl Pts',(119.53611361456,122.432001213286,65.3215459358927));
#21607=CARTESIAN_POINT('Ctrl Pts',(120.463214920894,121.172228781595,65.1448437142406));
#21608=CARTESIAN_POINT('Ctrl Pts',(121.375933771032,119.901950188821,64.9644538185964));
#21609=CARTESIAN_POINT('Ctrl Pts',(122.433881518173,118.429548939232,64.7553608611377));
#21610=CARTESIAN_POINT('Ctrl Pts',(123.472473810833,116.943050420668,64.5413290851279));
#21611=CARTESIAN_POINT('Ctrl Pts',(124.491680181692,115.442410467452,64.3225371850261));
#21612=CARTESIAN_POINT('Ctrl Pts',(125.503830307995,113.952159855199,64.1052600411091));
#21613=CARTESIAN_POINT('Ctrl Pts',(126.496862295989,112.447962781688,63.8832882990187));
#21614=CARTESIAN_POINT('Ctrl Pts',(127.470711714623,110.929748092818,63.6567711904821));
#21615=CARTESIAN_POINT('Ctrl Pts',(127.83402354599,110.363351123772,63.5722649578308));
#21616=CARTESIAN_POINT('Ctrl Pts',(128.194665186969,109.795002921474,63.4871258563392));
#21617=CARTESIAN_POINT('Ctrl Pts',(128.552631924842,109.224698859508,63.4013607746513));
#21618=CARTESIAN_POINT('Ctrl Pts',(129.336349318664,107.976099015325,63.2135902943521));
#21619=CARTESIAN_POINT('Ctrl Pts',(130.107456590396,106.717775301267,63.0227682840443));
#21620=CARTESIAN_POINT('Ctrl Pts',(130.865437062443,105.450406778866,62.8290762477486));
#21621=CARTESIAN_POINT('Ctrl Pts',(131.211808809534,104.871261714447,62.740565459564));
#21622=CARTESIAN_POINT('Ctrl Pts',(131.555439991089,104.290228375938,62.6514554438038));
#21623=CARTESIAN_POINT('Ctrl Pts',(131.896284148027,103.707373770585,62.5617639394275));
#21624=CARTESIAN_POINT('Ctrl Pts',(132.769178417835,102.214696150074,62.332066000863));
#21625=CARTESIAN_POINT('Ctrl Pts',(133.621557467831,100.71390800504,62.0991453921073));
#21626=CARTESIAN_POINT('Ctrl Pts',(134.453641402604,99.2050793476407,61.8631619225103));
#21627=CARTESIAN_POINT('Ctrl Pts',(134.657478130989,98.8354595480436,61.8053527323728));
#21628=CARTESIAN_POINT('Ctrl Pts',(134.860096801376,98.4653570557965,61.7473596212806));
#21629=CARTESIAN_POINT('Ctrl Pts',(135.061500391748,98.0947725661239,61.6891847168399));
#21630=CARTESIAN_POINT('Ctrl Pts',(135.918476370644,96.517928751097,61.4416494291702));
#21631=CARTESIAN_POINT('Ctrl Pts',(136.753474751504,94.9323379967978,61.1908139275639));
#21632=CARTESIAN_POINT('Ctrl Pts',(137.566662089513,93.3380809660457,60.9368477650047));
#21633=CARTESIAN_POINT('Ctrl Pts',(138.380360599555,91.742821780475,60.6827219585432));
#21634=CARTESIAN_POINT('Ctrl Pts',(139.172220905911,90.1388852411411,60.4254614269076));
#21635=CARTESIAN_POINT('Ctrl Pts',(139.942377264237,88.5263181774426,60.1652136179345));
#21636=CARTESIAN_POINT('Ctrl Pts',(140.712233804798,86.914378877507,59.9050671220462));
#21637=CARTESIAN_POINT('Ctrl Pts',(141.460403539085,85.2938155678344,59.6419355415775));
#21638=CARTESIAN_POINT('Ctrl Pts',(142.186984131365,83.6646439519117,59.3759457057129));
#21639=CARTESIAN_POINT('Ctrl Pts',(142.912502334737,82.0378544720814,59.110344793877));
#21640=CARTESIAN_POINT('Ctrl Pts',(143.616494706017,80.4024816159027,58.8418938423145));
#21641=CARTESIAN_POINT('Ctrl Pts',(144.299018648534,78.758513255544,58.5707007575231));
#21642=CARTESIAN_POINT('Ctrl Pts',(144.830588555321,77.4781418961833,58.3594875328673));
#21643=CARTESIAN_POINT('Ctrl Pts',(145.349135473784,76.1925561244661,58.1466106118989));
#21644=CARTESIAN_POINT('Ctrl Pts',(145.85466847965,74.9017398842795,57.9321140413525));
#21645=CARTESIAN_POINT('Ctrl Pts',(146.516232013982,73.2125189152811,57.6514140521017));
#21646=CARTESIAN_POINT('Ctrl Pts',(147.155497232843,71.5143630118513,57.3679509334573));
#21647=CARTESIAN_POINT('Ctrl Pts',(147.772428977714,69.807239987182,57.0818271781275));
#21648=CARTESIAN_POINT('Ctrl Pts',(148.386770152708,68.1072853754217,56.7969048905253));
#21649=CARTESIAN_POINT('Ctrl Pts',(148.978965174465,66.398438517869,56.5093441244595));
#21650=CARTESIAN_POINT('Ctrl Pts',(149.548932147378,64.6806505934696,56.2192337314343));
#21651=CARTESIAN_POINT('Ctrl Pts',(149.749721271601,64.0755047704084,56.1170330522513));
#21652=CARTESIAN_POINT('Ctrl Pts',(149.947751397002,63.4692492021539,56.0145158552573));
#21653=CARTESIAN_POINT('Ctrl Pts',(150.1430174875,62.8618813470188,55.911685707308));
#21654=CARTESIAN_POINT('Ctrl Pts',(150.692594437047,61.1524428458079,55.6222699726696));
#21655=CARTESIAN_POINT('Ctrl Pts',(151.220279633146,59.4341937070619,55.3303766976904));
#21656=CARTESIAN_POINT('Ctrl Pts',(151.725928605588,57.7070595737709,55.0360816657165));
#21657=CARTESIAN_POINT('Ctrl Pts',(151.821168551398,57.3817505743925,54.9806506366331));
#21658=CARTESIAN_POINT('Ctrl Pts',(151.915626585807,57.0561263418963,54.9251343787327));
#21659=CARTESIAN_POINT('Ctrl Pts',(152.009301540551,56.7301863473222,54.8695333676534));
#21660=CARTESIAN_POINT('Ctrl Pts',(152.264011555342,55.8439283174525,54.7183495811949));
#21661=CARTESIAN_POINT('Ctrl Pts',(152.513007414861,54.9550568431241,54.5664917271939));
#21662=CARTESIAN_POINT('Ctrl Pts',(152.755993471224,54.0645582860792,54.4141395690049));
#21663=CARTESIAN_POINT('Ctrl Pts',(152.998916131407,53.1742920642056,54.261827160195));
#21664=CARTESIAN_POINT('Ctrl Pts',(153.23583207891,52.2823997307104,54.1090207462948));
#21665=CARTESIAN_POINT('Ctrl Pts',(153.466495510062,51.3898821467467,53.9559047087908));
#21666=CARTESIAN_POINT('Ctrl Pts',(153.540466822289,51.1036612380325,53.9068020219861));
#21667=CARTESIAN_POINT('Ctrl Pts',(153.613795499395,50.8173761372881,53.8576675269881));
#21668=CARTESIAN_POINT('Ctrl Pts',(153.686474525376,50.5310601534892,53.8085073975534));
#21669=CARTESIAN_POINT('Ctrl Pts',(154.128896893156,48.7881557353863,53.5092526872527));
#21670=CARTESIAN_POINT('Ctrl Pts',(154.547717548931,47.0422790819696,53.2087305243606));
#21671=CARTESIAN_POINT('Ctrl Pts',(154.943135950867,45.2934692031631,52.9070433704346));
#21672=CARTESIAN_POINT('Ctrl Pts',(155.339941312342,43.538525243262,52.6042980263133));
#21673=CARTESIAN_POINT('Ctrl Pts',(155.713180124024,41.7806271784725,52.3003793805853));
#21674=CARTESIAN_POINT('Ctrl Pts',(156.063008646656,40.0197906561065,51.9953791652994));
#21675=CARTESIAN_POINT('Ctrl Pts',(156.413237885962,38.2569371553939,51.6900295826407));
#21676=CARTESIAN_POINT('Ctrl Pts',(156.740003301058,36.4911381757485,51.3835958217297));
#21677=CARTESIAN_POINT('Ctrl Pts',(157.043414214413,34.7223897964007,51.0761600223204));
#21678=CARTESIAN_POINT('Ctrl Pts',(157.34707364086,32.9521926981324,50.7684724131767));
#21679=CARTESIAN_POINT('Ctrl Pts',(157.627340398481,31.1790410720362,50.4597809926956));
#21680=CARTESIAN_POINT('Ctrl Pts',(157.884274805064,29.402915704594,50.1501601383299));
#21681=CARTESIAN_POINT('Ctrl Pts',(158.073892018425,28.0921378012609,49.9216604041597));
#21682=CARTESIAN_POINT('Ctrl Pts',(158.250800442238,26.7797399355903,49.6926542872569));
#21683=CARTESIAN_POINT('Ctrl Pts',(158.415006661951,25.4657104901417,49.463169537153));
#21684=CARTESIAN_POINT('Ctrl Pts',(158.639828857533,23.6666130777445,49.148971539896));
#21685=CARTESIAN_POINT('Ctrl Pts',(158.840838866152,21.8644778479518,48.8338827881402));
#21686=CARTESIAN_POINT('Ctrl Pts',(159.01800742211,20.0592853583608,48.5179779687453));
#21687=CARTESIAN_POINT('Ctrl Pts',(159.194796131046,18.2579631774022,48.2027504450717));
#21688=CARTESIAN_POINT('Ctrl Pts',(159.347845539902,16.4535965187214,47.8867102164476));
#21689=CARTESIAN_POINT('Ctrl Pts',(159.477074839366,14.6461632758025,47.5699289235262));
#21690=CARTESIAN_POINT('Ctrl Pts',(159.521446942324,14.0255639668495,47.4611590686801));
#21691=CARTESIAN_POINT('Ctrl Pts',(159.563010305271,13.4046031180388,47.3523018323499));
#21692=CARTESIAN_POINT('Ctrl Pts',(159.60176023808,12.7832798613223,47.2433600880803));
#21693=CARTESIAN_POINT('Ctrl Pts',(159.713375040897,10.9936284282252,46.929565703839));
#21694=CARTESIAN_POINT('Ctrl Pts',(159.801651714041,9.20096871886184,46.6150701364191));
#21695=CARTESIAN_POINT('Ctrl Pts',(159.866444427471,7.40526826756703,46.2999402754388));
#21696=CARTESIAN_POINT('Ctrl Pts',(159.878482139281,7.07164858436365,46.2413929134261));
#21697=CARTESIAN_POINT('Ctrl Pts',(159.889709106815,6.73792395991809,46.182823660671));
#21698=CARTESIAN_POINT('Ctrl Pts',(159.900124197961,6.40409421188559,46.1242329519068));
#21699=CARTESIAN_POINT('Ctrl Pts',(159.933361240614,5.33876377760979,45.937256010576));
#21700=CARTESIAN_POINT('Ctrl Pts',(159.958330637681,4.27236229656624,45.7500604690855));
#21701=CARTESIAN_POINT('Ctrl Pts',(159.974991372694,3.20488185158275,45.5626601505172));
#21702=CARTESIAN_POINT('Ctrl Pts',(159.9833217402,2.67114162909094,45.468959991233));
#21703=CARTESIAN_POINT('Ctrl Pts',(159.989574840371,2.13713166462133,45.3752086357616));
#21704=CARTESIAN_POINT('Ctrl Pts',(159.993744929012,1.60285087169006,45.2814078106192));
#21705=CARTESIAN_POINT('Ctrl Pts',(159.995829973332,1.33571047522442,45.234507398048));
#21706=CARTESIAN_POINT('Ctrl Pts',(159.997394258275,1.0685023715434,45.1875946178656));
#21707=CARTESIAN_POINT('Ctrl Pts',(159.998437026632,0.80122642143114,45.1406696856376));
#21708=CARTESIAN_POINT('Ctrl Pts',(159.999479794988,0.533950471318885,45.0937447534096));
#21709=CARTESIAN_POINT('Ctrl Pts',(160.,0.265592952447147,45.0466296899014));
#21710=CARTESIAN_POINT('Ctrl Pts',(160.,3.36777869765522E-14,45.));
#21711=CARTESIAN_POINT('Ctrl Pts',(65.4243934602224,173.04853626372,69.9999998857046));
#21712=CARTESIAN_POINT('Ctrl Pts',(56.5824686834193,149.661031129524,69.9968988863329));
#21713=CARTESIAN_POINT('Ctrl Pts',(56.5812975378023,149.661473897575,94.9999996631391));
#21714=CARTESIAN_POINT('Ctrl Pts',(69.2022850192574,170.614767694469,70.0001026648394));
#21715=CARTESIAN_POINT('Ctrl Pts',(60.0163277184471,148.362786737093,70.9204251271389));
#21716=CARTESIAN_POINT('Ctrl Pts',(60.4989568014547,148.180355676071,95.0002407754135));
#21717=CARTESIAN_POINT('Ctrl Pts',(72.867487114648,168.080831911,69.9354862567983));
#21718=CARTESIAN_POINT('Ctrl Pts',(63.529881785745,146.900483832406,71.6775178358105));
#21719=CARTESIAN_POINT('Ctrl Pts',(64.3290816927398,146.556845898137,94.871040775192));
#21720=CARTESIAN_POINT('Ctrl Pts',(79.9886618889852,162.815535315842,69.6989874325338));
#21721=CARTESIAN_POINT('Ctrl Pts',(70.5057678662081,143.683924978654,72.8662379282042));
#21722=CARTESIAN_POINT('Ctrl Pts',(71.8188031734396,143.035546027714,94.3981030531638));
#21723=CARTESIAN_POINT('Ctrl Pts',(83.4448180787027,160.084321402834,69.5270912439842));
#21724=CARTESIAN_POINT('Ctrl Pts',(73.9797811265126,141.934709130391,73.3100631633681));
#21725=CARTESIAN_POINT('Ctrl Pts',(75.4785580886896,141.137975699511,94.0543379212644));
#21726=CARTESIAN_POINT('Ctrl Pts',(90.1649508888079,154.418488187676,69.0903834186758));
#21727=CARTESIAN_POINT('Ctrl Pts',(80.8468574617034,138.140544889064,73.9275707376667));
#21728=CARTESIAN_POINT('Ctrl Pts',(82.6353585459653,137.070560054605,93.180971287852));
#21729=CARTESIAN_POINT('Ctrl Pts',(93.4288956283072,151.483876143982,68.8255110458721));
#21730=CARTESIAN_POINT('Ctrl Pts',(84.250544779031,136.099279342344,74.1094550058665));
#21731=CARTESIAN_POINT('Ctrl Pts',(86.1323917334847,134.9007094904,92.6512484049633));
#21732=CARTESIAN_POINT('Ctrl Pts',(98.1868895196157,146.923477254202,68.3655653196807));
#21733=CARTESIAN_POINT('Ctrl Pts',(89.3086164492795,132.791122112537,74.2087035772314));
#21734=CARTESIAN_POINT('Ctrl Pts',(91.2562278085006,131.440284798265,91.7313856490923));
#21735=CARTESIAN_POINT('Ctrl Pts',(99.7498644441552,145.376897980895,68.2017775273551));
#21736=CARTESIAN_POINT('Ctrl Pts',(90.9728032557208,131.658236954755,74.2136476432942));
#21737=CARTESIAN_POINT('Ctrl Pts',(92.9438609765903,130.252495749627,91.4038190220956));
#21738=CARTESIAN_POINT('Ctrl Pts',(102.830397761921,142.229443429941,67.8540969995271));
#21739=CARTESIAN_POINT('Ctrl Pts',(94.2736611523608,129.316493185164,74.1697160096125));
#21740=CARTESIAN_POINT('Ctrl Pts',(96.2782413450362,127.80756701287,90.7084745843661));
#21741=CARTESIAN_POINT('Ctrl Pts',(104.340526689813,140.636086286616,67.6710267247838));
#21742=CARTESIAN_POINT('Ctrl Pts',(95.9037030178137,128.113362455015,74.1215224810223));
#21743=CARTESIAN_POINT('Ctrl Pts',(97.9169503291095,126.556249426087,90.3423416598691));
#21744=CARTESIAN_POINT('Ctrl Pts',(108.773784815397,135.80766015676,67.0972794963739));
#21745=CARTESIAN_POINT('Ctrl Pts',(100.689275594125,124.436982180208,73.9049733062588));
#21746=CARTESIAN_POINT('Ctrl Pts',(102.73863706313,122.725817074548,89.194868194963));
#21747=CARTESIAN_POINT('Ctrl Pts',(111.604568491427,132.519638863472,66.6816419373888));
#21748=CARTESIAN_POINT('Ctrl Pts',(103.806017905932,121.852642889054,73.6651628390201));
#21749=CARTESIAN_POINT('Ctrl Pts',(105.832302044554,120.066719009531,88.3636043219205));
#21750=CARTESIAN_POINT('Ctrl Pts',(117.032367731531,125.801765879975,65.791893690712));
#21751=CARTESIAN_POINT('Ctrl Pts',(109.828742610535,116.451539928799,73.0190491317221));
#21752=CARTESIAN_POINT('Ctrl Pts',(111.787252032969,114.543020095861,86.5841254176761));
#21753=CARTESIAN_POINT('Ctrl Pts',(119.62934181667,122.371918899055,65.3177549901836));
#21754=CARTESIAN_POINT('Ctrl Pts',(112.74472984579,113.63381946986,72.615217563022));
#21755=CARTESIAN_POINT('Ctrl Pts',(114.648510013565,111.6784057416,85.6358543715796));
#21756=CARTESIAN_POINT('Ctrl Pts',(124.599146009151,115.364277479383,64.3161618719215));
#21757=CARTESIAN_POINT('Ctrl Pts',(118.360419512033,107.768760881291,71.6629242936508));
#21758=CARTESIAN_POINT('Ctrl Pts',(120.142754803448,105.745286540605,83.6326763250999));
#21759=CARTESIAN_POINT('Ctrl Pts',(126.971956044848,111.786495074342,63.7886914051919));
#21760=CARTESIAN_POINT('Ctrl Pts',(121.068699600671,104.720063055232,71.1159985294063));
#21761=CARTESIAN_POINT('Ctrl Pts',(122.775732250521,102.676780126252,82.5777372262751));
#21762=CARTESIAN_POINT('Ctrl Pts',(129.80075461093,107.216308621383,63.0980550220973));
#21763=CARTESIAN_POINT('Ctrl Pts',(124.331930740369,100.74355600257,70.3475688232352));
#21764=CARTESIAN_POINT('Ctrl Pts',(125.924058053992,98.7124951748074,81.1964639412214));
#21765=CARTESIAN_POINT('Ctrl Pts',(130.359642034789,106.297366146314,62.9583586603758));
#21766=CARTESIAN_POINT('Ctrl Pts',(124.974276453257,99.9453785304544,70.1907346207442));
#21767=CARTESIAN_POINT('Ctrl Pts',(126.546567681517,97.9131968052432,80.9170710194551));
#21768=CARTESIAN_POINT('Ctrl Pts',(131.463698410258,104.449503828761,62.6758629251867));
#21769=CARTESIAN_POINT('Ctrl Pts',(126.245180402254,98.3344969993201,69.8692369403547));
#21770=CARTESIAN_POINT('Ctrl Pts',(127.777227456477,96.3016513053162,80.3520788936282));
#21771=CARTESIAN_POINT('Ctrl Pts',(132.009235466058,103.519919452344,62.5329597002741));
#21772=CARTESIAN_POINT('Ctrl Pts',(126.874283999707,97.5211676540206,69.7044590655436));
#21773=CARTESIAN_POINT('Ctrl Pts',(128.38578921301,95.488818477239,80.0662719859412));
#21774=CARTESIAN_POINT('Ctrl Pts',(133.619372483136,100.726336503739,62.1012543515074));
#21775=CARTESIAN_POINT('Ctrl Pts',(128.730630620049,95.0726690744142,69.2014135825394));
#21776=CARTESIAN_POINT('Ctrl Pts',(130.183236617943,93.0399172816863,79.202859577207));
#21777=CARTESIAN_POINT('Ctrl Pts',(134.65924893846,98.8546953904331,61.8090337480645));
#21778=CARTESIAN_POINT('Ctrl Pts',(129.936019779115,93.4178260914866,68.8522667873865));
#21779=CARTESIAN_POINT('Ctrl Pts',(131.345830830391,91.3910083774188,78.6184167040672));
#21780=CARTESIAN_POINT('Ctrl Pts',(139.695933192192,89.4486190475415,60.3271033697907));
#21781=CARTESIAN_POINT('Ctrl Pts',(135.733435509069,85.1282711403168,67.062675590899));
#21782=CARTESIAN_POINT('Ctrl Pts',(136.984252256805,83.0663208160601,75.6545459910273));
#21783=CARTESIAN_POINT('Ctrl Pts',(143.208042277038,81.7712744795915,59.0755984870333));
#21784=CARTESIAN_POINT('Ctrl Pts',(139.892479129903,78.114080631359,65.4234070469369));
#21785=CARTESIAN_POINT('Ctrl Pts',(140.93966573095,76.1514359803153,73.1515201301065));
#21786=CARTESIAN_POINT('Ctrl Pts',(147.752894591533,69.9881927629273,57.1141792462043));
#21787=CARTESIAN_POINT('Ctrl Pts',(145.300074704311,67.1397517789991,62.7372455796463));
#21788=CARTESIAN_POINT('Ctrl Pts',(146.0744422133,65.4065361919382,69.2286486638968));
#21789=CARTESIAN_POINT('Ctrl Pts',(149.146622556606,66.0158544859077,56.4462099795947));
#21790=CARTESIAN_POINT('Ctrl Pts',(146.96016515084,63.4242781036387,61.8087879512217));
#21791=CARTESIAN_POINT('Ctrl Pts',(147.652339743588,61.762547280548,67.8926978272171));
#21792=CARTESIAN_POINT('Ctrl Pts',(151.056362852687,59.9840340597369,55.4238420750756));
#21793=CARTESIAN_POINT('Ctrl Pts',(149.242347721897,57.7367729866036,60.3647058331654));
#21794=CARTESIAN_POINT('Ctrl Pts',(149.817529237813,56.2019959846749,65.8479415997114));
#21795=CARTESIAN_POINT('Ctrl Pts',(151.662764458627,57.9611955519339,55.0796443921211));
#21796=CARTESIAN_POINT('Ctrl Pts',(149.967111817518,55.8263294589246,59.8759432129804));
#21797=CARTESIAN_POINT('Ctrl Pts',(150.50561314431,54.3327017344974,65.1595391420191));
#21798=CARTESIAN_POINT('Ctrl Pts',(152.526890246365,54.9076662578491,54.558287841893));
#21799=CARTESIAN_POINT('Ctrl Pts',(151.001777270768,52.931823465264,59.1304989048559));
#21800=CARTESIAN_POINT('Ctrl Pts',(151.486795724971,51.5048176135938,64.1168149427384));
#21801=CARTESIAN_POINT('Ctrl Pts',(152.807586251953,53.8857006221939,54.3835026198272));
#21802=CARTESIAN_POINT('Ctrl Pts',(151.337862433964,51.9624117285674,58.8800286279954));
#21803=CARTESIAN_POINT('Ctrl Pts',(151.805631706264,50.5573531931399,63.7672407289973));
#21804=CARTESIAN_POINT('Ctrl Pts',(153.352185443809,51.8411536782466,54.0332742455136));
#21805=CARTESIAN_POINT('Ctrl Pts',(151.990284568509,50.020368862806,58.37674383573));
#21806=CARTESIAN_POINT('Ctrl Pts',(152.424429813258,48.6599319331303,63.0667763221949));
#21807=CARTESIAN_POINT('Ctrl Pts',(153.616167010543,50.8183589242819,53.8577952672846));
#21808=CARTESIAN_POINT('Ctrl Pts',(152.30677555528,49.0474544806264,58.1238602884326));
#21809=CARTESIAN_POINT('Ctrl Pts',(152.724480699868,47.7097795578358,62.7158144756579));
#21810=CARTESIAN_POINT('Ctrl Pts',(155.917931196388,41.6079957482047,52.2752944335229));
#21811=CARTESIAN_POINT('Ctrl Pts',(155.053646875237,40.3201454128714,55.8492067253227));
#21812=CARTESIAN_POINT('Ctrl Pts',(155.34153850921,39.1455096493191,59.5507777164435));
#21813=CARTESIAN_POINT('Ctrl Pts',(157.440541638506,33.3840425923826,50.8461835808945));
#21814=CARTESIAN_POINT('Ctrl Pts',(156.901981554525,32.3845089234026,53.7374746717279));
#21815=CARTESIAN_POINT('Ctrl Pts',(157.078106276928,31.4415608589374,56.6925206006809));
#21816=CARTESIAN_POINT('Ctrl Pts',(158.971479743602,20.9484526935852,48.6740963454106));
#21817=CARTESIAN_POINT('Ctrl Pts',(158.754292373091,20.3422965289589,50.5031839548515));
#21818=CARTESIAN_POINT('Ctrl Pts',(158.825192956881,19.7505414459351,52.3482901787236));
#21819=CARTESIAN_POINT('Ctrl Pts',(159.355678878882,16.7866326262453,47.9452859172134));
#21820=CARTESIAN_POINT('Ctrl Pts',(159.219812677019,16.305216939573,49.413970141234));
#21821=CARTESIAN_POINT('Ctrl Pts',(159.263969037536,15.8309336665831,50.8906501976363));
#21822=CARTESIAN_POINT('Ctrl Pts',(159.741443596581,10.5129289469729,46.8452406498883));
#21823=CARTESIAN_POINT('Ctrl Pts',(159.686873998274,10.2140889507991,47.7668807512895));
#21824=CARTESIAN_POINT('Ctrl Pts',(159.704601275429,9.91705122717507,48.690530528023));
#21825=CARTESIAN_POINT('Ctrl Pts',(159.83823957573,8.41652647465408,46.4774188977111));
#21826=CARTESIAN_POINT('Ctrl Pts',(159.804111416692,8.17781928499459,47.2156464811373));
#21827=CARTESIAN_POINT('Ctrl Pts',(159.81518566301,7.9400062771006,47.9548772375799));
#21828=CARTESIAN_POINT('Ctrl Pts',(159.967567107828,4.21229224956273,45.7395342706948));
#21829=CARTESIAN_POINT('Ctrl Pts',(159.960706191155,4.09363866390366,46.1094110069741));
#21830=CARTESIAN_POINT('Ctrl Pts',(159.962941406069,3.97424771515215,46.4790883103916));
#21831=CARTESIAN_POINT('Ctrl Pts',(160.,2.10288127196593,45.3691939815787));
#21832=CARTESIAN_POINT('Ctrl Pts',(160.,2.04346271816514,45.5537959647716));
#21833=CARTESIAN_POINT('Ctrl Pts',(160.,1.98404404900769,45.7383979488414));
#21834=CARTESIAN_POINT('Ctrl Pts',(160.,0.,45.));
#21835=CARTESIAN_POINT('Ctrl Pts',(160.,0.,45.));
#21836=CARTESIAN_POINT('Ctrl Pts',(160.,0.,45.));
#21837=CARTESIAN_POINT('Origin',(65.4347826086958,173.041293409847,95.));
#21838=CARTESIAN_POINT('Origin',(0.,0.,95.));
#21839=CARTESIAN_POINT('Origin',(-14.5652173913043,184.425742352699,95.));
#21840=CARTESIAN_POINT('Ctrl Pts',(-12.5969447708577,159.503344737469,95.));
#21841=CARTESIAN_POINT('Ctrl Pts',(-12.5969447708577,159.503344737469,70.));
#21842=CARTESIAN_POINT('Ctrl Pts',(-14.5652173913043,184.425742352699,70.));
#21843=CARTESIAN_POINT('Ctrl Pts',(-16.5078129272362,159.194479802674,95.));
#21844=CARTESIAN_POINT('Ctrl Pts',(-15.9020915295028,159.242317288254,68.9408032477129));
#21845=CARTESIAN_POINT('Ctrl Pts',(-18.4950032706578,185.155983850241,70.));
#21846=CARTESIAN_POINT('Ctrl Pts',(-20.3710100863973,158.744819305304,94.8172074050833));
#21847=CARTESIAN_POINT('Ctrl Pts',(-18.9874545935604,158.899342445268,67.6784855507893));
#21848=CARTESIAN_POINT('Ctrl Pts',(-22.4253844615201,185.7615463294,69.908603702539));
#21849=CARTESIAN_POINT('Ctrl Pts',(-28.0013011400224,157.577989715187,94.060173223671));
#21850=CARTESIAN_POINT('Ctrl Pts',(-24.7902939337038,158.128801235359,64.714494728495));
#21851=CARTESIAN_POINT('Ctrl Pts',(-30.2945131193187,186.732665530968,69.5300866118382));
#21852=CARTESIAN_POINT('Ctrl Pts',(-31.7684865197378,156.860742338829,93.4863288792126));
#21853=CARTESIAN_POINT('Ctrl Pts',(-27.4990355473887,157.695444326737,62.9860517551233));
#21854=CARTESIAN_POINT('Ctrl Pts',(-34.2333599633667,187.09818816358,69.2431644395594));
#21855=CARTESIAN_POINT('Ctrl Pts',(-37.343678752542,155.592679657295,92.2879046923386));
#21856=CARTESIAN_POINT('Ctrl Pts',(-31.1436763210525,157.073827933375,60.0699145363268));
#21857=CARTESIAN_POINT('Ctrl Pts',(-40.1512716292601,187.470074489004,68.6439523461928));
#21858=CARTESIAN_POINT('Ctrl Pts',(-39.1894418276195,155.137945593457,91.8318643970813));
#21859=CARTESIAN_POINT('Ctrl Pts',(-32.3097589079898,156.867332358696,59.0181216219914));
#21860=CARTESIAN_POINT('Ctrl Pts',(-42.12548806774,187.564605345407,68.4159321985189));
#21861=CARTESIAN_POINT('Ctrl Pts',(-41.9382629795998,154.408810392036,91.0538818796549));
#21862=CARTESIAN_POINT('Ctrl Pts',(-33.9340426077785,156.58074776089,57.3545260494391));
#21863=CARTESIAN_POINT('Ctrl Pts',(-45.0892214588785,187.662475916888,68.0269409398383));
#21864=CARTESIAN_POINT('Ctrl Pts',(-42.8512294298429,154.157926593345,90.7788716538768));
#21865=CARTESIAN_POINT('Ctrl Pts',(-34.4599536442302,156.48817082939,56.7786869254312));
#21866=CARTESIAN_POINT('Ctrl Pts',(-46.0775309162799,187.687777109309,67.889435826931));
#21867=CARTESIAN_POINT('Ctrl Pts',(-44.6703555627358,153.640663657467,90.1955588967012));
#21868=CARTESIAN_POINT('Ctrl Pts',(-35.4696360776896,156.313503350392,55.593044712447));
#21869=CARTESIAN_POINT('Ctrl Pts',(-48.0549067566625,187.723758078197,67.597779448358));
#21870=CARTESIAN_POINT('Ctrl Pts',(-45.5780239544002,153.373821576854,89.8867032935461));
#21871=CARTESIAN_POINT('Ctrl Pts',(-35.9536596323359,156.231426864416,54.9814880064992));
#21872=CARTESIAN_POINT('Ctrl Pts',(-49.0456292326158,187.734439396951,67.4433516467711));
#21873=CARTESIAN_POINT('Ctrl Pts',(-48.2791863488088,152.553799743575,88.9109268015102));
#21874=CARTESIAN_POINT('Ctrl Pts',(-37.3406875913855,156.005960339725,53.0878622163732));
#21875=CARTESIAN_POINT('Ctrl Pts',(-52.006426339423,187.744558869217,66.9554634007591));
#21876=CARTESIAN_POINT('Ctrl Pts',(-50.0455010806815,151.982872872988,88.1971446848615));
#21877=CARTESIAN_POINT('Ctrl Pts',(-38.149975496957,155.888609930498,51.7769554149645));
#21878=CARTESIAN_POINT('Ctrl Pts',(-53.9592290714755,187.722159051229,66.5985723423992));
#21879=CARTESIAN_POINT('Ctrl Pts',(-53.5069789484465,150.799035238803,86.6315720785634));
#21880=CARTESIAN_POINT('Ctrl Pts',(-39.5296138424305,155.747546552728,49.058766931388));
#21881=CARTESIAN_POINT('Ctrl Pts',(-57.8192032663729,187.623216674501,65.8157860393133));
#21882=CARTESIAN_POINT('Ctrl Pts',(-55.2021601069382,150.186106336222,85.7798428475361));
#21883=CARTESIAN_POINT('Ctrl Pts',(-40.0921001658277,155.727065431804,47.6468076105207));
#21884=CARTESIAN_POINT('Ctrl Pts',(-59.7264018532888,187.546662547939,65.3899214237434));
#21885=CARTESIAN_POINT('Ctrl Pts',(-58.5174766142274,148.925652416265,83.9219691980032));
#21886=CARTESIAN_POINT('Ctrl Pts',(-40.9305626227692,155.823418532223,44.7505274971452));
#21887=CARTESIAN_POINT('Ctrl Pts',(-63.4894147199849,187.343877463659,64.4609845990262));
#21888=CARTESIAN_POINT('Ctrl Pts',(-60.1376466369853,148.278097849358,82.9159377469876));
#21889=CARTESIAN_POINT('Ctrl Pts',(-41.1959635800001,155.945547490035,43.261778192548));
#21890=CARTESIAN_POINT('Ctrl Pts',(-65.3452788129041,187.217628898092,63.9579688734417));
#21891=CARTESIAN_POINT('Ctrl Pts',(-62.5068712240698,147.2875546711,81.2731565607321));
#21892=CARTESIAN_POINT('Ctrl Pts',(-41.329056222797,156.271451344433,41.0337957981935));
#21893=CARTESIAN_POINT('Ctrl Pts',(-68.0836879900484,186.994915337258,63.1365782803921));
#21894=CARTESIAN_POINT('Ctrl Pts',(-63.2864190238013,146.954186749042,80.7032055873364));
#21895=CARTESIAN_POINT('Ctrl Pts',(-41.3272321247111,156.407028503944,40.2806421489842));
#21896=CARTESIAN_POINT('Ctrl Pts',(-68.9888958579059,186.915128162852,62.8516027936408));
#21897=CARTESIAN_POINT('Ctrl Pts',(-64.8239857104685,146.282448409019,79.514506063713));
#21898=CARTESIAN_POINT('Ctrl Pts',(-41.2235309507544,156.736842986134,38.7791997063422));
#21899=CARTESIAN_POINT('Ctrl Pts',(-70.7824898970565,186.745236566641,62.257253031884));
#21900=CARTESIAN_POINT('Ctrl Pts',(-65.5807923985165,145.944570108018,78.8965035406746));
#21901=CARTESIAN_POINT('Ctrl Pts',(-41.1193059140031,156.932266944476,38.0321782287653));
#21902=CARTESIAN_POINT('Ctrl Pts',(-71.669484323248,186.655232604801,61.9482517703102));
#21903=CARTESIAN_POINT('Ctrl Pts',(-67.795210035115,144.935989315356,76.9821802471142));
#21904=CARTESIAN_POINT('Ctrl Pts',(-40.6409532007916,157.620893025833,35.8178318542641));
#21905=CARTESIAN_POINT('Ctrl Pts',(-74.2765779917833,186.374146071458,60.9910901236114));
#21906=CARTESIAN_POINT('Ctrl Pts',(-69.2040289876185,144.267167110464,75.62063975569));
#21907=CARTESIAN_POINT('Ctrl Pts',(-40.0961119414972,158.21220805087,34.4207109664872));
#21908=CARTESIAN_POINT('Ctrl Pts',(-75.951232725749,186.171160493749,60.3103198777859));
#21909=CARTESIAN_POINT('Ctrl Pts',(-71.2069497472747,143.283368159876,73.4306585921975));
#21910=CARTESIAN_POINT('Ctrl Pts',(-38.9366264227514,159.316107000538,32.5645400570154));
#21911=CARTESIAN_POINT('Ctrl Pts',(-78.3523532248388,185.852751159626,59.2153292961283));
#21912=CARTESIAN_POINT('Ctrl Pts',(-71.856153509367,142.958707172039,72.6759694271163));
#21913=CARTESIAN_POINT('Ctrl Pts',(-38.4828035089153,159.728767083945,31.9784787713152));
#21914=CARTESIAN_POINT('Ctrl Pts',(-79.1341783828994,185.74431020609,58.8379847135414));
#21915=CARTESIAN_POINT('Ctrl Pts',(-73.1153413914611,142.318816769507,71.1125766454393));
#21916=CARTESIAN_POINT('Ctrl Pts',(-37.4500708169756,160.636987281432,30.9149848733693));
#21917=CARTESIAN_POINT('Ctrl Pts',(-80.6569760131837,185.524679875126,58.0562883227365));
#21918=CARTESIAN_POINT('Ctrl Pts',(-73.7253342774642,142.003581480544,70.3038873576441));
#21919=CARTESIAN_POINT('Ctrl Pts',(-36.8684153167661,161.134321354495,30.4403150385843));
#21920=CARTESIAN_POINT('Ctrl Pts',(-81.3979600403437,185.413487572967,57.6519436787834));
#21921=CARTESIAN_POINT('Ctrl Pts',(-74.9029624412775,141.385955049099,68.6265804660936));
#21922=CARTESIAN_POINT('Ctrl Pts',(-35.5797893182526,162.213781149297,29.6428068354536));
#21923=CARTESIAN_POINT('Ctrl Pts',(-82.8342463013922,185.190488834526,56.8132902330855));
#21924=CARTESIAN_POINT('Ctrl Pts',(-75.4717796014841,141.082897321633,67.755569241579));
#21925=CARTESIAN_POINT('Ctrl Pts',(-34.8681706018876,162.799215603146,29.3240421033952));
#21926=CARTESIAN_POINT('Ctrl Pts',(-83.5310202701526,185.078415158267,56.3777846207694));
#21927=CARTESIAN_POINT('Ctrl Pts',(-76.5472441445947,140.502287692226,65.9735353866643));
#21928=CARTESIAN_POINT('Ctrl Pts',(-33.3511237074772,164.031531871629,28.8970199109168));
#21929=CARTESIAN_POINT('Ctrl Pts',(-84.8533571151316,184.859437149692,55.4867676933523));
#21930=CARTESIAN_POINT('Ctrl Pts',(-77.0558663375507,140.223721881846,65.0600083704848));
#21931=CARTESIAN_POINT('Ctrl Pts',(-32.5426488911884,164.680643187567,28.7922370175357));
#21932=CARTESIAN_POINT('Ctrl Pts',(-85.4813144285751,184.752179051019,55.0300041852196));
#21933=CARTESIAN_POINT('Ctrl Pts',(-78.0120454916522,139.694020894368,63.1847493041814));
#21934=CARTESIAN_POINT('Ctrl Pts',(-30.8564359524551,166.023964520988,28.8369857496512));
#21935=CARTESIAN_POINT('Ctrl Pts',(-86.6658003364468,184.544904934636,54.0923746521136));
#21936=CARTESIAN_POINT('Ctrl Pts',(-78.4596142273092,139.44287884185,62.2230271057913));
#21937=CARTESIAN_POINT('Ctrl Pts',(-29.9787416594907,166.717911624714,28.9922485335044));
#21938=CARTESIAN_POINT('Ctrl Pts',(-87.2223435128929,184.444886160955,53.6115135528724));
#21939=CARTESIAN_POINT('Ctrl Pts',(-79.2896319659011,138.972593654695,60.2472126840058));
#21940=CARTESIAN_POINT('Ctrl Pts',(-28.1983849287021,168.118768320068,29.6042074660882));
#21941=CARTESIAN_POINT('Ctrl Pts',(-88.2574884412621,184.255114157391,52.6236063420261));
#21942=CARTESIAN_POINT('Ctrl Pts',(-79.672099531494,138.753440210982,59.2331358058206));
#21943=CARTESIAN_POINT('Ctrl Pts',(-27.297364480468,168.824245091024,30.0665548817476));
#21944=CARTESIAN_POINT('Ctrl Pts',(-88.7361129449165,184.165357043077,52.1165679028911));
#21945=CARTESIAN_POINT('Ctrl Pts',(-80.1926695171554,138.45279307131,57.668598294985));
#21946=CARTESIAN_POINT('Ctrl Pts',(-25.9814571746451,169.851558160624,31.0113827393965));
#21947=CARTESIAN_POINT('Ctrl Pts',(-89.3891560196825,184.04094680916,51.3342991475022));
#21948=CARTESIAN_POINT('Ctrl Pts',(-80.3577007193496,138.3570444551,57.1383954883763));
#21949=CARTESIAN_POINT('Ctrl Pts',(-25.5454666502937,170.191393781686,31.3722996228226));
#21950=CARTESIAN_POINT('Ctrl Pts',(-89.5964791741451,184.001090877233,51.0691977441812));
#21951=CARTESIAN_POINT('Ctrl Pts',(-80.6659819895472,138.177534950197,56.0739089930283));
#21952=CARTESIAN_POINT('Ctrl Pts',(-24.7029234986323,170.847361230438,32.1739158547286));
#21953=CARTESIAN_POINT('Ctrl Pts',(-89.9842031495538,183.926020864336,50.5369544965211));
#21954=CARTESIAN_POINT('Ctrl Pts',(-80.8095563275921,138.093589167787,55.5388388898697));
#21955=CARTESIAN_POINT('Ctrl Pts',(-24.2962688576142,171.163570352953,32.6151710790885));
#21956=CARTESIAN_POINT('Ctrl Pts',(-90.1650091326306,183.890731563919,50.2694194449313));
#21957=CARTESIAN_POINT('Ctrl Pts',(-81.2084719518345,137.859635628646,53.9250716815212));
#21958=CARTESIAN_POINT('Ctrl Pts',(-23.1286439767822,172.070717278649,34.0596081714576));
#21959=CARTESIAN_POINT('Ctrl Pts',(-90.6678576024157,183.792000424905,49.4625358407677));
#21960=CARTESIAN_POINT('Ctrl Pts',(-81.4320538801261,137.727501177533,52.8378286338531));
#21961=CARTESIAN_POINT('Ctrl Pts',(-22.4329377587908,172.610133759847,35.1736153870478));
#21962=CARTESIAN_POINT('Ctrl Pts',(-90.9503795006326,183.735700011795,48.9189143169189));
#21963=CARTESIAN_POINT('Ctrl Pts',(-81.792814884011,137.513560833443,50.639890051958));
#21964=CARTESIAN_POINT('Ctrl Pts',(-21.2676444399461,173.512933127601,37.6575994990932));
#21965=CARTESIAN_POINT('Ctrl Pts',(-91.4067479064495,183.644151612346,47.8199450259868));
#21966=CARTESIAN_POINT('Ctrl Pts',(-81.9300025600908,137.431751226209,49.5291966979117));
#21967=CARTESIAN_POINT('Ctrl Pts',(-20.803417489149,173.872150439349,39.0242467263608));
#21968=CARTESIAN_POINT('Ctrl Pts',(-91.5806039650975,183.608903080856,47.2645983489531));
#21969=CARTESIAN_POINT('Ctrl Pts',(-82.1146690690122,137.321493904945,47.2833282524998));
#21970=CARTESIAN_POINT('Ctrl Pts',(-20.16786749127,174.363820312557,41.9243194792464));
#21971=CARTESIAN_POINT('Ctrl Pts',(-91.8147222258894,183.561326025264,46.1416641262527));
#21972=CARTESIAN_POINT('Ctrl Pts',(-82.1621621619488,137.293041006723,46.1481485313624));
#21973=CARTESIAN_POINT('Ctrl Pts',(-20.0000000006397,174.493598372083,43.4505009035421));
#21974=CARTESIAN_POINT('Ctrl Pts',(-91.8749999997178,183.54899720507,45.5740742656792));
#21975=CARTESIAN_POINT('Ctrl Pts',(-82.1621621621622,137.293041006595,45.0000000000001));
#21976=CARTESIAN_POINT('Ctrl Pts',(-20.0000000000001,174.493598372593,45.));
#21977=CARTESIAN_POINT('Ctrl Pts',(-91.875,183.548997205106,45.0000000000001));
#21978=CARTESIAN_POINT('Ctrl Pts',(-82.1621621621622,137.293041006595,-45.));
#21979=CARTESIAN_POINT('Ctrl Pts',(-20.,174.493598372593,-45.));
#21980=CARTESIAN_POINT('Ctrl Pts',(-91.875,183.548997205106,-45.));
#21981=CARTESIAN_POINT('Ctrl Pts',(-82.1621621620694,137.29304100665,-46.1481557420891));
#21982=CARTESIAN_POINT('Ctrl Pts',(-20.0000000008088,174.493598372051,-43.4504962324451));
#21983=CARTESIAN_POINT('Ctrl Pts',(-91.8749999998195,183.548997205083,-45.5740778710447));
#21984=CARTESIAN_POINT('Ctrl Pts',(-82.1146674891305,137.321494909959,-47.2836204764629));
#21985=CARTESIAN_POINT('Ctrl Pts',(-20.1678750458358,174.363814523666,-41.9239156869814));
#21986=CARTESIAN_POINT('Ctrl Pts',(-91.8147201804456,183.561326491592,-46.1418102382312));
#21987=CARTESIAN_POINT('Ctrl Pts',(-81.9298687787757,137.431831040152,-49.5305505033));
#21988=CARTESIAN_POINT('Ctrl Pts',(-20.8038733338462,173.87179773671,-39.0225342454562));
#21989=CARTESIAN_POINT('Ctrl Pts',(-91.5804344010687,183.608937488634,-47.2652752516501));
#21990=CARTESIAN_POINT('Ctrl Pts',(-81.7925509092854,137.513718286535,-50.6420203314529));
#21991=CARTESIAN_POINT('Ctrl Pts',(-21.2685350175652,173.512244042647,-37.6549923514553));
#21992=CARTESIAN_POINT('Ctrl Pts',(-91.4064133506295,183.64421947132,-47.8210101657326));
#21993=CARTESIAN_POINT('Ctrl Pts',(-81.4312911519869,137.727952582462,-52.8419520617065));
#21994=CARTESIAN_POINT('Ctrl Pts',(-22.4353472619568,172.608266146777,-35.1691826276842));
#21995=CARTESIAN_POINT('Ctrl Pts',(-90.9494152627793,183.73589269126,-48.9209760308471));
#21996=CARTESIAN_POINT('Ctrl Pts',(-81.2073409782417,137.86030323698,-53.930411905424));
#21997=CARTESIAN_POINT('Ctrl Pts',(-23.1321166236791,172.068023990567,-34.0542643968245));
#21998=CARTESIAN_POINT('Ctrl Pts',(-90.6664290227458,183.792284465073,-49.4652059527151));
#21999=CARTESIAN_POINT('Ctrl Pts',(-80.8076155883356,138.094725179005,-55.5463038168551));
#22000=CARTESIAN_POINT('Ctrl Pts',(-24.3018243019137,171.159251906869,-32.608821652411));
#22001=CARTESIAN_POINT('Ctrl Pts',(-90.1625642421299,183.891209812319,-50.273151908426));
#22002=CARTESIAN_POINT('Ctrl Pts',(-80.6637284362082,138.178851055812,-56.0821321396214));
#22003=CARTESIAN_POINT('Ctrl Pts',(-24.7092393480367,170.8424484307,-32.1672993257694));
#22004=CARTESIAN_POINT('Ctrl Pts',(-89.9813662332113,183.926573325791,-50.5410660698153));
#22005=CARTESIAN_POINT('Ctrl Pts',(-80.3547223160008,138.358774806128,-57.1482305947251));
#22006=CARTESIAN_POINT('Ctrl Pts',(-25.5534323448973,170.185187553971,-31.3653336068408));
#22007=CARTESIAN_POINT('Ctrl Pts',(-89.5927359269015,184.001812393928,-51.0741152973578));
#22008=CARTESIAN_POINT('Ctrl Pts',(-80.1897157463767,138.454503844763,-57.6778553276653));
#22009=CARTESIAN_POINT('Ctrl Pts',(-25.9891497436588,169.845558624407,-31.0053311458501));
#22010=CARTESIAN_POINT('Ctrl Pts',(-89.3854472959172,184.041657349327,-51.3389276638432));
#22011=CARTESIAN_POINT('Ctrl Pts',(-79.6691857343974,138.755113166885,-59.2411239335854));
#22012=CARTESIAN_POINT('Ctrl Pts',(-27.3043824228755,168.818754356815,-30.0625716779723));
#22013=CARTESIAN_POINT('Ctrl Pts',(-88.7324643102342,184.166044042608,-52.1205619667716));
#22014=CARTESIAN_POINT('Ctrl Pts',(-79.2865367003683,138.974361582824,-60.2551804226534));
#22015=CARTESIAN_POINT('Ctrl Pts',(-28.2054764565281,168.113208434832,-29.6008985931059));
#22016=CARTESIAN_POINT('Ctrl Pts',(-88.2536187741394,184.2558352071,-52.6275902113403));
#22017=CARTESIAN_POINT('Ctrl Pts',(-78.4554952448704,139.44519835826,-62.2322272830292));
#22018=CARTESIAN_POINT('Ctrl Pts',(-29.9870871732745,166.711325253611,-28.9902411417199));
#22019=CARTESIAN_POINT('Ctrl Pts',(-87.2172161146977,184.445814432147,-53.616113641501));
#22020=CARTESIAN_POINT('Ctrl Pts',(-78.0070853906616,139.696796360684,-63.1952037501853));
#22021=CARTESIAN_POINT('Ctrl Pts',(-30.8659062634836,166.016465199281,-28.8356077015459));
#22022=CARTESIAN_POINT('Ctrl Pts',(-86.6596376820301,184.54600608238,-54.0976018751081));
#22023=CARTESIAN_POINT('Ctrl Pts',(-77.048374490535,140.227844142847,-65.0739651883141));
#22024=CARTESIAN_POINT('Ctrl Pts',(-32.5550498620837,164.670719156008,-28.7930246590335));
#22025=CARTESIAN_POINT('Ctrl Pts',(-85.4720522235598,184.753776814215,-55.0369825941415));
#22026=CARTESIAN_POINT('Ctrl Pts',(-76.5380623346242,140.507300416309,-65.9897411795777));
#22027=CARTESIAN_POINT('Ctrl Pts',(-33.3652850012716,164.020134276596,-28.8993088042511));
#22028=CARTESIAN_POINT('Ctrl Pts',(-84.8420314669778,184.861358481738,-55.4948705898156));
#22029=CARTESIAN_POINT('Ctrl Pts',(-75.728170044288,140.944451383507,-67.3302212152897));
#22030=CARTESIAN_POINT('Ctrl Pts',(-34.5122899170826,163.088248299172,-29.2247287175038));
#22031=CARTESIAN_POINT('Ctrl Pts',(-83.8462836568007,185.026184135095,-56.1651106076315));
#22032=CARTESIAN_POINT('Ctrl Pts',(-75.4504275008882,141.093358021468,-67.7720166440731));
#22033=CARTESIAN_POINT('Ctrl Pts',(-34.8806149643643,162.787129232841,-29.3592240626014));
#22034=CARTESIAN_POINT('Ctrl Pts',(-83.5054586515878,185.081771633102,-56.3860083220514));
#22035=CARTESIAN_POINT('Ctrl Pts',(-74.8846583831958,141.394450480466,-68.638474298271));
#22036=CARTESIAN_POINT('Ctrl Pts',(-35.5848353719522,162.207090776343,-29.6738942085392));
#22037=CARTESIAN_POINT('Ctrl Pts',(-82.8126262261615,185.192937470074,-56.8192371491206));
#22038=CARTESIAN_POINT('Ctrl Pts',(-74.5961940186673,141.546875246922,-69.0639054241725));
#22039=CARTESIAN_POINT('Ctrl Pts',(-35.9216661334723,161.92746439315,-29.8536204285411));
#22040=CARTESIAN_POINT('Ctrl Pts',(-82.4600788359989,185.248607363413,-57.0319527121015));
#22041=CARTESIAN_POINT('Ctrl Pts',(-73.7147852409945,142.009051309513,-70.3181048368547));
#22042=CARTESIAN_POINT('Ctrl Pts',(-36.8788387621073,161.125452934343,-30.448321955934));
#22043=CARTESIAN_POINT('Ctrl Pts',(-81.3851340173047,185.415427325518,-57.6590524183968));
#22044=CARTESIAN_POINT('Ctrl Pts',(-73.1058526825644,142.323686171231,-71.1248228832094));
#22045=CARTESIAN_POINT('Ctrl Pts',(-37.4586012957459,160.629612122475,-30.9226581436019));
#22046=CARTESIAN_POINT('Ctrl Pts',(-80.6454711362611,185.526378252561,-58.0624114416317));
#22047=CARTESIAN_POINT('Ctrl Pts',(-71.8484094427491,142.962594416718,-72.6851127793295));
#22048=CARTESIAN_POINT('Ctrl Pts',(-38.4884482750362,159.723677205105,-31.9853928652137));
#22049=CARTESIAN_POINT('Ctrl Pts',(-79.1248432297244,185.745617009401,-58.8425563896376));
#22050=CARTESIAN_POINT('Ctrl Pts',(-71.1998903691279,143.28687342725,-73.4386712566775));
#22051=CARTESIAN_POINT('Ctrl Pts',(-38.9412443107916,159.311835992123,-32.571024190995));
#22052=CARTESIAN_POINT('Ctrl Pts',(-78.3438671457771,185.853907640827,-59.2193356283638));
#22053=CARTESIAN_POINT('Ctrl Pts',(-69.1983701639693,144.269870406751,-75.6262347306282));
#22054=CARTESIAN_POINT('Ctrl Pts',(-40.098518501438,158.209672336637,-34.4263336337102));
#22055=CARTESIAN_POINT('Ctrl Pts',(-75.9444956785313,186.171991112866,-60.313117365264));
#22056=CARTESIAN_POINT('Ctrl Pts',(-67.789611337796,144.938619930464,-76.9874494541838));
#22057=CARTESIAN_POINT('Ctrl Pts',(-40.6428501902966,157.618722485761,-35.8233464689691));
#22058=CARTESIAN_POINT('Ctrl Pts',(-74.2699390339847,186.374928413795,-60.9937247271315));
#22059=CARTESIAN_POINT('Ctrl Pts',(-65.5736968005695,145.947761291759,-78.9024214954926));
#22060=CARTESIAN_POINT('Ctrl Pts',(-41.1204746256597,156.930311424546,-38.039180340206));
#22061=CARTESIAN_POINT('Ctrl Pts',(-71.6611543736691,186.656097205558,-61.9512107477265));
#22062=CARTESIAN_POINT('Ctrl Pts',(-64.8158802459753,146.286035214527,-79.5209801538095));
#22063=CARTESIAN_POINT('Ctrl Pts',(-41.2244105509083,156.734894047821,-38.7871825470194));
#22064=CARTESIAN_POINT('Ctrl Pts',(-70.7730084836254,186.746172400419,-62.2604900769237));
#22065=CARTESIAN_POINT('Ctrl Pts',(-63.2798154046224,146.957025668062,-80.708101155254));
#22066=CARTESIAN_POINT('Ctrl Pts',(-41.3273505057767,156.405812865881,-40.28705578889));
#22067=CARTESIAN_POINT('Ctrl Pts',(-68.9812191627737,186.915817204625,-62.854050577608));
#22068=CARTESIAN_POINT('Ctrl Pts',(-62.5011418348097,147.28997967661,-81.2772464428291));
#22069=CARTESIAN_POINT('Ctrl Pts',(-41.3289113131743,156.270545080631,-41.0393070509114));
#22070=CARTESIAN_POINT('Ctrl Pts',(-68.0770491726709,186.995479791273,-63.1386232214322));
#22071=CARTESIAN_POINT('Ctrl Pts',(-60.1349066172685,148.279183910951,-82.9176021366126));
#22072=CARTESIAN_POINT('Ctrl Pts',(-41.1954499968666,155.945365284604,-43.2643582639517));
#22073=CARTESIAN_POINT('Ctrl Pts',(-65.3421452709541,187.21783448214,-63.9588010682709));
#22074=CARTESIAN_POINT('Ctrl Pts',(-58.5172177905218,148.925716472836,-83.9220069329356));
#22075=CARTESIAN_POINT('Ctrl Pts',(-40.9303152653076,155.823488084658,-44.7507715365026));
#22076=CARTESIAN_POINT('Ctrl Pts',(-63.4891393214523,187.343863770612,-64.4610034664955));
#22077=CARTESIAN_POINT('Ctrl Pts',(-55.2078389271008,150.183981588884,-85.7767676195814));
#22078=CARTESIAN_POINT('Ctrl Pts',(-40.0936579164813,155.727150148364,-47.6420141653999));
#22079=CARTESIAN_POINT('Ctrl Pts',(-59.7328291881618,187.546344672458,-65.388383809763));
#22080=CARTESIAN_POINT('Ctrl Pts',(-53.5161142772202,150.795743533889,-86.6270094856871));
#22081=CARTESIAN_POINT('Ctrl Pts',(-39.532641345483,155.7474211318,-49.0512964022449));
#22082=CARTESIAN_POINT('Ctrl Pts',(-57.8294753314208,187.622813755709,-65.8135047428673));
#22083=CARTESIAN_POINT('Ctrl Pts',(-50.0625427301627,151.977210695096,-88.1898645846761));
#22084=CARTESIAN_POINT('Ctrl Pts',(-38.1572551119495,155.887688976429,-51.7640573981651));
#22085=CARTESIAN_POINT('Ctrl Pts',(-53.9781482037484,187.721812660418,-66.5949322923142));
#22086=CARTESIAN_POINT('Ctrl Pts',(-48.300677812312,152.546933899424,-88.902415984378));
#22087=CARTESIAN_POINT('Ctrl Pts',(-37.3506839361543,156.004473544864,-53.0722212299062));
#22088=CARTESIAN_POINT('Ctrl Pts',(-52.0301478787376,187.744353908368,-66.9512079922001));
#22089=CARTESIAN_POINT('Ctrl Pts',(-45.6069622945489,153.365203420054,-89.8766149078073));
#22090=CARTESIAN_POINT('Ctrl Pts',(-35.968800254378,156.228899730153,-54.9617694105439));
#22091=CARTESIAN_POINT('Ctrl Pts',(-49.0772687551371,187.734687416337,-67.438307453898));
#22092=CARTESIAN_POINT('Ctrl Pts',(-44.6988593852777,153.632385143467,-90.1860654079167));
#22093=CARTESIAN_POINT('Ctrl Pts',(-35.4850829390786,156.310864009055,-55.574055857639));
#22094=CARTESIAN_POINT('Ctrl Pts',(-48.085971399696,187.724177624307,-67.5930327039756));
#22095=CARTESIAN_POINT('Ctrl Pts',(-42.8761650692597,154.151004745895,-90.7712192710136));
#22096=CARTESIAN_POINT('Ctrl Pts',(-34.4741829322119,156.485677849815,-56.7627908597524));
#22097=CARTESIAN_POINT('Ctrl Pts',(-46.1045568957785,187.688410388535,-67.8856096354897));
#22098=CARTESIAN_POINT('Ctrl Pts',(-41.961505308882,154.402506184776,-91.0470382563051));
#22099=CARTESIAN_POINT('Ctrl Pts',(-33.9476129855026,156.57835701425,-57.340037903017));
#22100=CARTESIAN_POINT('Ctrl Pts',(-45.1143442223383,187.663188471079,-68.0235191281666));
#22101=CARTESIAN_POINT('Ctrl Pts',(-39.2078728242664,155.133330023901,-91.8271696738661));
#22102=CARTESIAN_POINT('Ctrl Pts',(-32.3213222389258,156.865285274486,-59.0074115145415));
#22103=CARTESIAN_POINT('Ctrl Pts',(-42.1452357351134,187.565487512066,-68.413584836905));
#22104=CARTESIAN_POINT('Ctrl Pts',(-37.3592600401471,155.588971030372,-92.2842750101778));
#22105=CARTESIAN_POINT('Ctrl Pts',(-31.1537789584207,157.072069906232,-60.0612788653556));
#22106=CARTESIAN_POINT('Ctrl Pts',(-40.1678814465501,187.470978958484,-68.6421375051228));
#22107=CARTESIAN_POINT('Ctrl Pts',(-31.7765730898505,156.859230747872,-93.4851484356314));
#22108=CARTESIAN_POINT('Ctrl Pts',(-27.5050829333197,157.694479721468,-62.9822688779818));
#22109=CARTESIAN_POINT('Ctrl Pts',(-34.2418029492231,187.098995873263,-69.2425742177477));
#22110=CARTESIAN_POINT('Ctrl Pts',(-28.0057930465495,157.577245982649,-94.0596464150218));
#22111=CARTESIAN_POINT('Ctrl Pts',(-24.7937282524838,158.12831660148,-64.712605314168));
#22112=CARTESIAN_POINT('Ctrl Pts',(-30.2991672680022,186.733191336003,-69.5298232075278));
#22113=CARTESIAN_POINT('Ctrl Pts',(-20.3711181309634,158.744859575788,-94.8172777838099));
#22114=CARTESIAN_POINT('Ctrl Pts',(-18.9876739109975,158.899340600304,-67.6785024920399));
#22115=CARTESIAN_POINT('Ctrl Pts',(-22.4254742611568,185.761605939772,-69.9086388918881));
#22116=CARTESIAN_POINT('Ctrl Pts',(-16.5071336512573,159.19453344921,-95.));
#22117=CARTESIAN_POINT('Ctrl Pts',(-15.9015003142952,159.242363980563,-68.9409927140224));
#22118=CARTESIAN_POINT('Ctrl Pts',(-18.4943215078181,185.15585716373,-70.));
#22119=CARTESIAN_POINT('Ctrl Pts',(-12.5969447708578,159.503344737469,-95.));
#22120=CARTESIAN_POINT('Ctrl Pts',(-12.5969447708578,159.503344737469,-70.));
#22121=CARTESIAN_POINT('Ctrl Pts',(-14.5652173913043,184.425742352699,-70.));
#22122=CARTESIAN_POINT('Origin',(-14.5652173913044,184.425742352699,-95.));
#22123=CARTESIAN_POINT('Origin',(0.,0.,-95.));
#22124=CARTESIAN_POINT('Origin',(65.4347826086956,173.041293409847,-95.));
#22125=CARTESIAN_POINT('Ctrl Pts',(56.5812969309658,149.661474126996,-94.999999663102));
#22126=CARTESIAN_POINT('Ctrl Pts',(56.5824681415181,149.661031334401,-69.9968987143965));
#22127=CARTESIAN_POINT('Ctrl Pts',(65.4243928842982,173.048536665204,-69.9999998856919));
#22128=CARTESIAN_POINT('Ctrl Pts',(60.4989564059575,148.180355843715,-95.0002407886545));
#22129=CARTESIAN_POINT('Ctrl Pts',(60.0163273489374,148.362786890788,-70.9204250223862));
#22130=CARTESIAN_POINT('Ctrl Pts',(69.2022846505335,170.614767979795,-70.0001026705298));
#22131=CARTESIAN_POINT('Ctrl Pts',(64.3290814992657,146.556845989099,-94.8710407874072));
#22132=CARTESIAN_POINT('Ctrl Pts',(63.5298815986881,146.90048391857,-71.6775177805552));
#22133=CARTESIAN_POINT('Ctrl Pts',(72.8674869407948,168.080832069929,-69.9354862610261));
#22134=CARTESIAN_POINT('Ctrl Pts',(71.8188031734667,143.035546027701,-94.3981030531637));
#22135=CARTESIAN_POINT('Ctrl Pts',(70.5057678650493,143.683924979291,-72.8662379072352));
#22136=CARTESIAN_POINT('Ctrl Pts',(79.9886618996876,162.815535337367,-69.6989874289698));
#22137=CARTESIAN_POINT('Ctrl Pts',(75.4785580886895,141.137975699511,-94.0543379212976));
#22138=CARTESIAN_POINT('Ctrl Pts',(73.9797811251018,141.934709131226,-73.3100631433763));
#22139=CARTESIAN_POINT('Ctrl Pts',(83.4448180894751,160.084321423497,-69.5270912396781));
#22140=CARTESIAN_POINT('Ctrl Pts',(82.6353585459652,137.070560054605,-93.1809712878189));
#22141=CARTESIAN_POINT('Ctrl Pts',(80.8468574599951,138.140544890001,-73.9275707196295));
#22142=CARTESIAN_POINT('Ctrl Pts',(90.1649508997293,154.41848820675,-69.0903834130075));
#22143=CARTESIAN_POINT('Ctrl Pts',(86.1323917334308,134.900709490437,-92.6512484049633));
#22144=CARTESIAN_POINT('Ctrl Pts',(84.2505447772597,136.099279343518,-74.1094549887923));
#22145=CARTESIAN_POINT('Ctrl Pts',(93.4288956391719,151.483876162247,-68.8255110396083));
#22146=CARTESIAN_POINT('Ctrl Pts',(91.2562278085275,131.440284798247,-91.7313856490923));
#22147=CARTESIAN_POINT('Ctrl Pts',(89.3086164475295,132.791122113729,-74.2087035613002));
#22148=CARTESIAN_POINT('Ctrl Pts',(98.1868895303702,146.923477271295,-68.3655653126085));
#22149=CARTESIAN_POINT('Ctrl Pts',(92.9438609765793,130.252495749635,-91.4038190221124));
#22150=CARTESIAN_POINT('Ctrl Pts',(90.9728032539421,131.658236956057,-74.2136476278089));
#22151=CARTESIAN_POINT('Ctrl Pts',(99.7498644548314,145.376897997586,-68.2017775200415));
#22152=CARTESIAN_POINT('Ctrl Pts',(96.2782413450471,127.807567012862,-90.7084745843493));
#22153=CARTESIAN_POINT('Ctrl Pts',(94.2736611505731,129.316493186476,-74.1697159948556));
#22154=CARTESIAN_POINT('Ctrl Pts',(102.830397772462,142.229443445845,-67.8540969917478));
#22155=CARTESIAN_POINT('Ctrl Pts',(97.9169503291257,126.556249426074,-90.3423416598691));
#22156=CARTESIAN_POINT('Ctrl Pts',(95.903703016047,128.113362456395,-74.1215224666304));
#22157=CARTESIAN_POINT('Ctrl Pts',(104.340526700227,140.636086302123,-67.67102671681));
#22158=CARTESIAN_POINT('Ctrl Pts',(102.738637063097,122.725817074573,-89.194868194963));
#22159=CARTESIAN_POINT('Ctrl Pts',(100.689275592308,124.436982181698,-73.9049732929621));
#22160=CARTESIAN_POINT('Ctrl Pts',(108.773784825643,135.807660171076,-67.0972794877753));
#22161=CARTESIAN_POINT('Ctrl Pts',(105.832302044602,120.066719009486,-88.3636043219205));
#22162=CARTESIAN_POINT('Ctrl Pts',(103.806017904117,121.852642890427,-73.6651628264369));
#22163=CARTESIAN_POINT('Ctrl Pts',(111.604568501322,132.519638876911,-66.6816419285586));
#22164=CARTESIAN_POINT('Ctrl Pts',(111.787252032921,114.543020095905,-86.5841254176761));
#22165=CARTESIAN_POINT('Ctrl Pts',(109.828742608944,116.451539930578,-73.0190491201399));
#22166=CARTESIAN_POINT('Ctrl Pts',(117.032367740893,125.801765892224,-65.7918936812914));
#22167=CARTESIAN_POINT('Ctrl Pts',(114.648510013566,111.678405741599,-85.6358543716459));
#22168=CARTESIAN_POINT('Ctrl Pts',(112.744729844124,113.633819471468,-72.6152175520978));
#22169=CARTESIAN_POINT('Ctrl Pts',(119.629341825712,122.371918910437,-65.3177549806292));
#22170=CARTESIAN_POINT('Ctrl Pts',(120.142754803447,105.745286540606,-83.6326763250335));
#22171=CARTESIAN_POINT('Ctrl Pts',(118.360419510627,107.768760882995,-71.6629242837753));
#22172=CARTESIAN_POINT('Ctrl Pts',(124.599146017412,115.364277489534,-64.3161618621584));
#22173=CARTESIAN_POINT('Ctrl Pts',(122.775732250518,102.676780126255,-82.5777372261749));
#22174=CARTESIAN_POINT('Ctrl Pts',(121.068699599138,104.720063056805,-71.1159985199901));
#22175=CARTESIAN_POINT('Ctrl Pts',(126.971956052825,111.786495083743,-63.7886913953421));
#22176=CARTESIAN_POINT('Ctrl Pts',(125.924058053993,98.7124951748066,-81.1964639412465));
#22177=CARTESIAN_POINT('Ctrl Pts',(124.331930739111,100.743556004242,-70.3475688144439));
#22178=CARTESIAN_POINT('Ctrl Pts',(129.800754618314,107.216308630159,-63.0980550122952));
#22179=CARTESIAN_POINT('Ctrl Pts',(126.546567681521,97.9131968052379,-80.9170710194467));
#22180=CARTESIAN_POINT('Ctrl Pts',(124.974276451984,99.9453785320827,-70.1907346120513));
#22181=CARTESIAN_POINT('Ctrl Pts',(130.35964204207,106.297366154906,-62.958358650597));
#22182=CARTESIAN_POINT('Ctrl Pts',(127.777227456473,96.3016513053215,-80.3520788936366));
#22183=CARTESIAN_POINT('Ctrl Pts',(126.245180401018,98.3344970009766,-69.8692369319056));
#22184=CARTESIAN_POINT('Ctrl Pts',(131.463698417375,104.449503837098,-62.6758629153771));
#22185=CARTESIAN_POINT('Ctrl Pts',(128.385789213004,95.488818477247,-80.0662719859161));
#22186=CARTESIAN_POINT('Ctrl Pts',(126.874283998473,97.5211676556489,-69.7044590571902));
#22187=CARTESIAN_POINT('Ctrl Pts',(132.009235473065,103.519919460513,-62.5329596904946));
#22188=CARTESIAN_POINT('Ctrl Pts',(130.183236617954,93.0399172816704,-79.2028595772572));
#22189=CARTESIAN_POINT('Ctrl Pts',(128.730630618919,95.0726690760594,-69.2014135745425));
#22190=CARTESIAN_POINT('Ctrl Pts',(133.619372489814,100.726336511492,-62.1012543417964));
#22191=CARTESIAN_POINT('Ctrl Pts',(131.345830830401,91.3910083774034,-78.6184167040505));
#22192=CARTESIAN_POINT('Ctrl Pts',(129.936019778023,93.4178260930886,-68.8522667795203));
#22193=CARTESIAN_POINT('Ctrl Pts',(134.659248944961,98.8546953978921,-61.8090337383792));
#22194=CARTESIAN_POINT('Ctrl Pts',(136.984252256763,83.066320816122,-75.6545459910939));
#22195=CARTESIAN_POINT('Ctrl Pts',(135.733435507954,85.1282711420036,-67.0626755844076));
#22196=CARTESIAN_POINT('Ctrl Pts',(139.69593319768,89.4486190536225,-60.3271033604134));
#22197=CARTESIAN_POINT('Ctrl Pts',(140.939665730898,76.1514359804232,-73.1515201298415));
#22198=CARTESIAN_POINT('Ctrl Pts',(139.892479128959,78.1140806329442,-65.4234070407235));
#22199=CARTESIAN_POINT('Ctrl Pts',(143.208042281703,81.7712744848519,-59.0755984780511));
#22200=CARTESIAN_POINT('Ctrl Pts',(146.074442213326,65.4065361918843,-69.2286486640292));
#22201=CARTESIAN_POINT('Ctrl Pts',(145.300074703784,67.1397517802941,-62.7372455747638));
#22202=CARTESIAN_POINT('Ctrl Pts',(147.752894595048,69.9881927669513,-57.1141792381744));
#22203=CARTESIAN_POINT('Ctrl Pts',(147.652339743601,61.7625472805127,-67.8926978272171));
#22204=CARTESIAN_POINT('Ctrl Pts',(146.960165150244,63.4242781048417,-61.8087879465894));
#22205=CARTESIAN_POINT('Ctrl Pts',(149.146622559743,66.0158544895779,-56.4462099719241));
#22206=CARTESIAN_POINT('Ctrl Pts',(149.817529237806,56.2019959846926,-65.8479415997114));
#22207=CARTESIAN_POINT('Ctrl Pts',(149.242347721494,57.7367729878032,-60.3647058289904));
#22208=CARTESIAN_POINT('Ctrl Pts',(151.056362855309,59.9840340630083,-55.4238420679245));
#22209=CARTESIAN_POINT('Ctrl Pts',(150.505613144304,54.3327017345152,-65.1595391420024));
#22210=CARTESIAN_POINT('Ctrl Pts',(149.967111817076,55.8263294600576,-59.8759432089222));
#22211=CARTESIAN_POINT('Ctrl Pts',(151.662764461086,57.9611955550307,-55.0796443851654));
#22212=CARTESIAN_POINT('Ctrl Pts',(151.486795724974,51.5048176135849,-64.1168149427468));
#22213=CARTESIAN_POINT('Ctrl Pts',(151.001777270418,52.9318234663437,-59.1304989011081));
#22214=CARTESIAN_POINT('Ctrl Pts',(152.526890248574,54.9076662607108,-54.5582878352699));
#22215=CARTESIAN_POINT('Ctrl Pts',(151.805631706267,50.5573531931324,-63.7672407289972));
#22216=CARTESIAN_POINT('Ctrl Pts',(151.337862433627,51.9624117296005,-58.8800286243506));
#22217=CARTESIAN_POINT('Ctrl Pts',(152.807586254088,53.8857006249786,-54.3835026132985));
#22218=CARTESIAN_POINT('Ctrl Pts',(152.424429813256,48.6599319331378,-63.0667763221948));
#22219=CARTESIAN_POINT('Ctrl Pts',(151.990284568165,50.0203688638623,-58.3767438321395));
#22220=CARTESIAN_POINT('Ctrl Pts',(153.352185445787,51.8411536809008,-54.0332742392006));
#22221=CARTESIAN_POINT('Ctrl Pts',(152.724480699873,47.7097795578204,-62.7158144756994));
#22222=CARTESIAN_POINT('Ctrl Pts',(152.306775554914,49.0474544815894,-58.1238602850607));
#22223=CARTESIAN_POINT('Ctrl Pts',(153.616167012447,50.8183589268311,-53.8577952610939));
#22224=CARTESIAN_POINT('Ctrl Pts',(155.341538509173,39.1455096494411,-59.5507777161094));
#22225=CARTESIAN_POINT('Ctrl Pts',(155.053646875419,40.3201454141209,-55.8492067218196));
#22226=CARTESIAN_POINT('Ctrl Pts',(155.917931197662,41.6079957503088,-52.2752944281586));
#22227=CARTESIAN_POINT('Ctrl Pts',(157.07810627687,31.4415608593237,-56.6925205993872));
#22228=CARTESIAN_POINT('Ctrl Pts',(156.90198155413,32.3845089243095,-53.737474669054));
#22229=CARTESIAN_POINT('Ctrl Pts',(157.44054163938,33.3840425942794,-50.8461835759691));
#22230=CARTESIAN_POINT('Ctrl Pts',(158.82519295691,19.7505414457421,-52.3482901793705));
#22231=CARTESIAN_POINT('Ctrl Pts',(158.754292373171,20.3422965292876,-50.5031839537118));
#22232=CARTESIAN_POINT('Ctrl Pts',(158.971479743882,20.9484526942674,-48.6740963430449));
#22233=CARTESIAN_POINT('Ctrl Pts',(159.263969037573,15.8309336660904,-50.8906501993346));
#22234=CARTESIAN_POINT('Ctrl Pts',(159.219812676319,16.3052169394273,-49.4139701412218));
#22235=CARTESIAN_POINT('Ctrl Pts',(159.355678879032,16.7866326264316,-47.9452859158802));
#22236=CARTESIAN_POINT('Ctrl Pts',(159.704601275411,9.91705122742161,-48.6905305271729));
#22237=CARTESIAN_POINT('Ctrl Pts',(159.686873998594,10.2140889512697,-47.7668807500635));
#22238=CARTESIAN_POINT('Ctrl Pts',(159.741443596687,10.5129289476784,-46.845240648104));
#22239=CARTESIAN_POINT('Ctrl Pts',(159.815185663009,7.94000627714555,-47.9548772374033));
#22240=CARTESIAN_POINT('Ctrl Pts',(159.804111417455,8.17781928521151,-47.2156464805718));
#22241=CARTESIAN_POINT('Ctrl Pts',(159.838239575783,8.41652647505475,-46.4774188965339));
#22242=CARTESIAN_POINT('Ctrl Pts',(159.962941406071,3.97424771510734,-46.4790883105662));
#22243=CARTESIAN_POINT('Ctrl Pts',(159.960706190386,4.09363866395126,-46.109411006716));
#22244=CARTESIAN_POINT('Ctrl Pts',(159.967567107836,4.21229224969148,-45.7395342702298));
#22245=CARTESIAN_POINT('Ctrl Pts',(160.,1.98404404958242,-45.7383979472562));
#22246=CARTESIAN_POINT('Ctrl Pts',(160.,2.04346271857147,-45.5537959634005));
#22247=CARTESIAN_POINT('Ctrl Pts',(160.,2.10288127222745,-45.3691939804612));
#22248=CARTESIAN_POINT('Ctrl Pts',(160.,0.,-45.));
#22249=CARTESIAN_POINT('Ctrl Pts',(160.,0.,-45.));
#22250=CARTESIAN_POINT('Ctrl Pts',(160.,0.,-45.));
#22251=CARTESIAN_POINT('Origin',(180.,-125.,85.));
#22252=CARTESIAN_POINT('',(180.,-137.5,73.9644660940673));
#22253=CARTESIAN_POINT('',(180.,-137.5,-73.9644660940672));
#22254=CARTESIAN_POINT('',(180.,-137.5,85.));
#22255=CARTESIAN_POINT('',(180.,-127.5,-73.9644660940672));
#22256=CARTESIAN_POINT('',(180.,-125.,-73.9644660940672));
#22257=CARTESIAN_POINT('',(180.,-127.5,73.9644660940673));
#22258=CARTESIAN_POINT('',(180.,-127.5,85.));
#22259=CARTESIAN_POINT('',(180.,-125.,73.9644660940673));
#22260=CARTESIAN_POINT('Origin',(180.,-140.,85.));
#22261=CARTESIAN_POINT('',(168.964466094067,-140.,82.5));
#22262=CARTESIAN_POINT('',(97.2111104761179,-140.,82.5));
#22263=CARTESIAN_POINT('',(180.,-140.,82.5));
#22264=CARTESIAN_POINT('',(97.2111104761179,-140.,-82.5));
#22265=CARTESIAN_POINT('',(97.2111104761179,-140.,85.));
#22266=CARTESIAN_POINT('',(168.964466094067,-140.,-82.5));
#22267=CARTESIAN_POINT('',(170.,-140.,-82.5));
#22268=CARTESIAN_POINT('',(177.5,-140.,-73.9644660940671));
#22269=CARTESIAN_POINT('',(258.232233047034,-140.,6.76776695296644));
#22270=CARTESIAN_POINT('',(177.5,-140.,73.9644660940673));
#22271=CARTESIAN_POINT('',(177.5,-140.,85.));
#22272=CARTESIAN_POINT('',(173.232233047034,-140.,78.2322330470336));
#22273=CARTESIAN_POINT('Origin',(0.,0.,85.));
#22274=CARTESIAN_POINT('',(104.163333279998,-137.5,85.));
#22275=CARTESIAN_POINT('',(168.964466094067,-137.5,85.));
#22276=CARTESIAN_POINT('',(0.,-137.5,85.));
#22277=CARTESIAN_POINT('',(168.964466094067,-127.5,85.));
#22278=CARTESIAN_POINT('',(168.964466094067,0.,85.));
#22279=CARTESIAN_POINT('',(116.189500386222,-127.5,85.));
#22280=CARTESIAN_POINT('',(0.,-127.5,85.));
#22281=CARTESIAN_POINT('Origin',(0.,0.,85.));
#22282=CARTESIAN_POINT('Origin',(0.,0.,-85.));
#22283=CARTESIAN_POINT('',(168.964466094067,-137.5,-85.));
#22284=CARTESIAN_POINT('',(104.163333279998,-137.5,-85.));
#22285=CARTESIAN_POINT('',(96.4365076099295,-137.5,-85.));
#22286=CARTESIAN_POINT('',(116.189500386223,-127.5,-85.));
#22287=CARTESIAN_POINT('Origin',(0.,0.,-85.));
#22288=CARTESIAN_POINT('',(168.964466094067,-127.5,-85.));
#22289=CARTESIAN_POINT('',(170.,-127.5,-85.));
#22290=CARTESIAN_POINT('',(168.964466094067,-140.,-85.));
#22291=CARTESIAN_POINT('Origin',(150.,-79.9999999999999,-47.));
#22292=CARTESIAN_POINT('',(150.,-122.5,-44.5));
#22293=CARTESIAN_POINT('',(150.,-80.6225774829854,-44.5));
#22294=CARTESIAN_POINT('',(150.,-79.9999999999999,-44.5));
#22295=CARTESIAN_POINT('',(150.,-80.6225774829854,-37.5));
#22296=CARTESIAN_POINT('',(150.,-80.6225774829854,-35.));
#22297=CARTESIAN_POINT('',(150.,-122.5,-37.5));
#22298=CARTESIAN_POINT('',(150.,-125.,-37.5));
#22299=CARTESIAN_POINT('',(150.,-122.5,-47.));
#22300=CARTESIAN_POINT('Origin',(0.,0.,-47.));
#22301=CARTESIAN_POINT('',(147.5,-122.5,-47.));
#22302=CARTESIAN_POINT('',(121.449578014911,-122.5,-47.));
#22303=CARTESIAN_POINT('',(0.,-122.5,-47.));
#22304=CARTESIAN_POINT('',(147.5,-89.4427190999916,-47.));
#22305=CARTESIAN_POINT('Origin',(0.,0.,-47.));
#22306=CARTESIAN_POINT('',(147.5,0.,-47.));
#22307=CARTESIAN_POINT('Origin',(0.,0.,-35.));
#22308=CARTESIAN_POINT('',(147.5,-122.5,-35.));
#22309=CARTESIAN_POINT('',(147.5,-89.4427190999916,-35.));
#22310=CARTESIAN_POINT('',(147.5,-79.9999999999999,-35.));
#22311=CARTESIAN_POINT('',(121.449578014911,-122.5,-35.));
#22312=CARTESIAN_POINT('Origin',(0.,0.,-35.));
#22313=CARTESIAN_POINT('',(150.,-122.5,-35.));
#22314=CARTESIAN_POINT('Origin',(150.,-79.9999999999999,47.));
#22315=CARTESIAN_POINT('',(150.,-122.5,37.5));
#22316=CARTESIAN_POINT('',(150.,-80.6225774829854,37.5));
#22317=CARTESIAN_POINT('',(150.,-79.9999999999999,37.5));
#22318=CARTESIAN_POINT('',(150.,-80.6225774829854,44.5));
#22319=CARTESIAN_POINT('',(150.,-80.6225774829854,47.));
#22320=CARTESIAN_POINT('',(150.,-122.5,44.5));
#22321=CARTESIAN_POINT('',(150.,-125.,44.5));
#22322=CARTESIAN_POINT('',(150.,-122.5,35.));
#22323=CARTESIAN_POINT('Origin',(0.,0.,47.));
#22324=CARTESIAN_POINT('',(147.5,-122.5,47.));
#22325=CARTESIAN_POINT('',(147.5,-89.4427190999916,47.));
#22326=CARTESIAN_POINT('',(147.5,-79.9999999999999,47.));
#22327=CARTESIAN_POINT('',(121.449578014911,-122.5,47.));
#22328=CARTESIAN_POINT('Origin',(0.,0.,47.));
#22329=CARTESIAN_POINT('',(0.,-122.5,47.));
#22330=CARTESIAN_POINT('Origin',(0.,0.,35.));
#22331=CARTESIAN_POINT('',(147.5,-122.5,35.));
#22332=CARTESIAN_POINT('',(121.449578014911,-122.5,35.));
#22333=CARTESIAN_POINT('',(115.217186218029,-122.5,35.));
#22334=CARTESIAN_POINT('',(147.5,-89.4427190999916,35.));
#22335=CARTESIAN_POINT('Origin',(0.,0.,35.));
#22336=CARTESIAN_POINT('',(147.5,0.,35.));
#22337=CARTESIAN_POINT('Origin',(-180.,-125.,85.));
#22338=CARTESIAN_POINT('',(-180.,-127.5,73.9644660940671));
#22339=CARTESIAN_POINT('',(-180.,-127.5,-73.9644660940673));
#22340=CARTESIAN_POINT('',(-180.,-127.5,85.));
#22341=CARTESIAN_POINT('',(-180.,-137.5,-73.9644660940673));
#22342=CARTESIAN_POINT('',(-180.,-140.,-73.9644660940673));
#22343=CARTESIAN_POINT('',(-180.,-137.5,73.9644660940671));
#22344=CARTESIAN_POINT('',(-180.,-137.5,85.));
#22345=CARTESIAN_POINT('',(-180.,-125.,73.9644660940671));
#22346=CARTESIAN_POINT('Origin',(0.,0.,85.));
#22347=CARTESIAN_POINT('',(-168.964466094067,-127.5,85.));
#22348=CARTESIAN_POINT('',(-168.964466094067,-137.5,85.));
#22349=CARTESIAN_POINT('',(-168.964466094067,0.,85.));
#22350=CARTESIAN_POINT('',(-104.163333279998,-137.5,85.));
#22351=CARTESIAN_POINT('',(-96.4365076099295,-137.5,85.));
#22352=CARTESIAN_POINT('',(-116.189500386222,-127.5,85.));
#22353=CARTESIAN_POINT('Origin',(0.,0.,85.));
#22354=CARTESIAN_POINT('',(-170.,-127.5,85.));
#22355=CARTESIAN_POINT('Origin',(0.,0.,-85.));
#22356=CARTESIAN_POINT('',(-168.964466094067,-127.5,-85.));
#22357=CARTESIAN_POINT('',(-116.189500386223,-127.5,-85.));
#22358=CARTESIAN_POINT('',(0.,-127.5,-85.));
#22359=CARTESIAN_POINT('',(-104.163333279998,-137.5,-85.));
#22360=CARTESIAN_POINT('Origin',(0.,0.,-85.));
#22361=CARTESIAN_POINT('',(-168.964466094067,-137.5,-85.));
#22362=CARTESIAN_POINT('',(0.,-137.5,-85.));
#22363=CARTESIAN_POINT('',(-168.964466094067,-125.,-85.));
#22364=CARTESIAN_POINT('Origin',(-150.,-79.9999999999999,-47.));
#22365=CARTESIAN_POINT('',(-150.,-122.5,-44.5));
#22366=CARTESIAN_POINT('',(-150.,-122.5,-37.5));
#22367=CARTESIAN_POINT('',(-150.,-122.5,-47.));
#22368=CARTESIAN_POINT('',(-150.,-80.6225774829854,-37.5));
#22369=CARTESIAN_POINT('',(-150.,-79.9999999999999,-37.5));
#22370=CARTESIAN_POINT('',(-150.,-80.6225774829854,-44.5));
#22371=CARTESIAN_POINT('',(-150.,-80.6225774829854,-47.));
#22372=CARTESIAN_POINT('',(-150.,-125.,-44.5));
#22373=CARTESIAN_POINT('Origin',(0.,0.,-47.));
#22374=CARTESIAN_POINT('',(-147.5,-122.5,-47.));
#22375=CARTESIAN_POINT('',(-147.5,-89.4427190999916,-47.));
#22376=CARTESIAN_POINT('',(-147.5,-79.9999999999999,-47.));
#22377=CARTESIAN_POINT('Origin',(0.,0.,-47.));
#22378=CARTESIAN_POINT('',(-150.,-122.5,-47.));
#22379=CARTESIAN_POINT('Origin',(0.,0.,-35.));
#22380=CARTESIAN_POINT('',(-147.5,-122.5,-35.));
#22381=CARTESIAN_POINT('',(0.,-122.5,-35.));
#22382=CARTESIAN_POINT('',(-147.5,-89.4427190999916,-35.));
#22383=CARTESIAN_POINT('Origin',(0.,0.,-35.));
#22384=CARTESIAN_POINT('',(-147.5,0.,-35.));
#22385=CARTESIAN_POINT('Origin',(-150.,-79.9999999999999,47.));
#22386=CARTESIAN_POINT('',(-150.,-122.5,37.5));
#22387=CARTESIAN_POINT('',(-150.,-122.5,44.5));
#22388=CARTESIAN_POINT('',(-150.,-122.5,47.));
#22389=CARTESIAN_POINT('',(-150.,-80.6225774829854,44.5));
#22390=CARTESIAN_POINT('',(-150.,-79.9999999999999,44.5));
#22391=CARTESIAN_POINT('',(-150.,-80.6225774829854,37.5));
#22392=CARTESIAN_POINT('',(-150.,-80.6225774829854,35.));
#22393=CARTESIAN_POINT('',(-150.,-125.,37.5));
#22394=CARTESIAN_POINT('Origin',(0.,0.,47.));
#22395=CARTESIAN_POINT('',(-147.5,-122.5,47.));
#22396=CARTESIAN_POINT('',(-115.217186218029,-122.5,47.));
#22397=CARTESIAN_POINT('',(-147.5,-89.4427190999916,47.));
#22398=CARTESIAN_POINT('Origin',(0.,0.,47.));
#22399=CARTESIAN_POINT('',(-147.5,0.,47.));
#22400=CARTESIAN_POINT('Origin',(0.,0.,35.));
#22401=CARTESIAN_POINT('',(-147.5,-122.5,35.));
#22402=CARTESIAN_POINT('',(-147.5,-89.4427190999916,35.));
#22403=CARTESIAN_POINT('',(-147.5,-79.9999999999999,35.));
#22404=CARTESIAN_POINT('Origin',(0.,0.,35.));
#22405=CARTESIAN_POINT('',(0.,-122.5,35.));
#22406=CARTESIAN_POINT('Origin',(-170.,0.,85.));
#22407=CARTESIAN_POINT('',(-170.732233047034,-127.5,84.2677669529664));
#22408=CARTESIAN_POINT('',(-179.267766952966,-127.5,75.7322330470335));
#22409=CARTESIAN_POINT('',(-180.,-127.5,74.9999999999999));
#22410=CARTESIAN_POINT('',(-179.267766952966,-137.5,75.7322330470335));
#22411=CARTESIAN_POINT('',(-179.267766952966,-140.,75.7322330470335));
#22412=CARTESIAN_POINT('',(-170.732233047034,-137.5,84.2677669529664));
#22413=CARTESIAN_POINT('',(-170.,-137.5,85.));
#22414=CARTESIAN_POINT('',(-170.732233047034,0.,84.2677669529664));
#22415=CARTESIAN_POINT('Origin',(-180.,-125.,-75.));
#22416=CARTESIAN_POINT('',(-179.267766952966,-127.5,-75.7322330470336));
#22417=CARTESIAN_POINT('',(-170.732233047034,-127.5,-84.2677669529664));
#22418=CARTESIAN_POINT('',(-170.,-127.5,-85.));
#22419=CARTESIAN_POINT('',(-170.732233047034,-137.5,-84.2677669529664));
#22420=CARTESIAN_POINT('',(-170.732233047034,-140.,-84.2677669529664));
#22421=CARTESIAN_POINT('',(-179.267766952966,-137.5,-75.7322330470336));
#22422=CARTESIAN_POINT('',(-180.,-137.5,-75.));
#22423=CARTESIAN_POINT('',(-179.267766952966,-125.,-75.7322330470336));
#22424=CARTESIAN_POINT('Origin',(180.,-125.,75.));
#22425=CARTESIAN_POINT('',(170.732233047034,-137.5,84.2677669529664));
#22426=CARTESIAN_POINT('',(179.267766952966,-137.5,75.7322330470336));
#22427=CARTESIAN_POINT('',(180.,-137.5,75.));
#22428=CARTESIAN_POINT('',(179.267766952966,-127.5,75.7322330470336));
#22429=CARTESIAN_POINT('',(179.267766952966,-125.,75.7322330470336));
#22430=CARTESIAN_POINT('',(170.732233047034,-127.5,84.2677669529664));
#22431=CARTESIAN_POINT('',(180.,-127.5,75.));
#22432=CARTESIAN_POINT('',(170.732233047034,-125.,84.2677669529664));
#22433=CARTESIAN_POINT('Origin',(170.,0.,-85.));
#22434=CARTESIAN_POINT('',(179.267766952966,-127.5,-75.7322330470335));
#22435=CARTESIAN_POINT('',(179.267766952966,-137.5,-75.7322330470335));
#22436=CARTESIAN_POINT('',(179.267766952966,0.,-75.7322330470335));
#22437=CARTESIAN_POINT('',(170.732233047034,-137.5,-84.2677669529664));
#22438=CARTESIAN_POINT('',(170.,-137.5,-85.));
#22439=CARTESIAN_POINT('',(170.732233047034,-127.5,-84.2677669529664));
#22440=CARTESIAN_POINT('',(170.732233047034,-125.,-84.2677669529664));
#22441=CARTESIAN_POINT('',(170.,-127.5,-85.));
#22442=CARTESIAN_POINT('Origin',(0.,0.,115.));
#22443=CARTESIAN_POINT('Origin',(0.,0.,125.));
#22444=CARTESIAN_POINT('Origin',(0.,-122.5,-49.5));
#22445=CARTESIAN_POINT('Origin',(-147.5,-122.5,-49.5));
#22446=CARTESIAN_POINT('Origin',(-147.5,-79.9999999999999,-44.5));
#22447=CARTESIAN_POINT('Ctrl Pts',(-147.5,-89.4427190999916,-47.));
#22448=CARTESIAN_POINT('Ctrl Pts',(-147.692029124167,-88.8093685912607,
-47.));
#22449=CARTESIAN_POINT('Ctrl Pts',(-147.881019325447,-88.1768396525117,
-46.9784293604652));
#22450=CARTESIAN_POINT('Ctrl Pts',(-148.067032921855,-87.5451886197927,
-46.9349710385975));
#22451=CARTESIAN_POINT('Ctrl Pts',(-148.113199638035,-87.3884191442505,
-46.9241851172987));
#22452=CARTESIAN_POINT('Ctrl Pts',(-148.159182993745,-87.2317038217232,
-46.9120507147773));
#22453=CARTESIAN_POINT('Ctrl Pts',(-148.204983936061,-87.075043664733,-46.8985625026983));
#22454=CARTESIAN_POINT('Ctrl Pts',(-148.227650188964,-86.9975147197269,
-46.8918873730891));
#22455=CARTESIAN_POINT('Ctrl Pts',(-148.250265804087,-86.9200215223737,
-46.8848824575639));
#22456=CARTESIAN_POINT('Ctrl Pts',(-148.272833473781,-86.8425552539348,
-46.877546723474));
#22457=CARTESIAN_POINT('Ctrl Pts',(-148.349179005414,-86.5804899398113,
-46.8527302259542));
#22458=CARTESIAN_POINT('Ctrl Pts',(-148.42497434185,-86.3187382386177,-46.8240687356948));
#22459=CARTESIAN_POINT('Ctrl Pts',(-148.500300623518,-86.0570314559301,
-46.7911753910845));
#22460=CARTESIAN_POINT('Ctrl Pts',(-148.548487711945,-85.8896146181409,
-46.7701331403549));
#22461=CARTESIAN_POINT('Ctrl Pts',(-148.596482723484,-85.7222162995132,
-46.7473581833852));
#22462=CARTESIAN_POINT('Ctrl Pts',(-148.644305530043,-85.5547679896948,
-46.7227381433699));
#22463=CARTESIAN_POINT('Ctrl Pts',(-148.705029122316,-85.3421484547092,
-46.6914765470896));
#22464=CARTESIAN_POINT('Ctrl Pts',(-148.765481316907,-85.1294146681287,
-46.6572181679748));
#22465=CARTESIAN_POINT('Ctrl Pts',(-148.825445173605,-84.9173615305767,
-46.6197236282395));
#22466=CARTESIAN_POINT('Ctrl Pts',(-148.844370664369,-84.8504343861742,
-46.6078897902489));
#22467=CARTESIAN_POINT('Ctrl Pts',(-148.863247416388,-84.7835753431854,
-46.5957333861149));
#22468=CARTESIAN_POINT('Ctrl Pts',(-148.882068323811,-84.7168103169457,
-46.5832463102145));
#22469=CARTESIAN_POINT('Ctrl Pts',(-148.922791444531,-84.5723496827009,
-46.5562278095707));
#22470=CARTESIAN_POINT('Ctrl Pts',(-148.963298334261,-84.4281714850036,
-46.5276326949765));
#22471=CARTESIAN_POINT('Ctrl Pts',(-149.003534667861,-84.2844711674245,
-46.4973441122003));
#22472=CARTESIAN_POINT('Ctrl Pts',(-149.04618468001,-84.1321506217299,-46.4652385919447));
#22473=CARTESIAN_POINT('Ctrl Pts',(-149.088661184858,-83.9798999176171,
-46.431152727177));
#22474=CARTESIAN_POINT('Ctrl Pts',(-149.130874866099,-83.8280577825329,
-46.3948300518332));
#22475=CARTESIAN_POINT('Ctrl Pts',(-149.153428770871,-83.7469316415657,
-46.3754235907832));
#22476=CARTESIAN_POINT('Ctrl Pts',(-149.175907457634,-83.6659227742882,
-46.3553781599173));
#22477=CARTESIAN_POINT('Ctrl Pts',(-149.198295785931,-83.5850879913779,
-46.3346512081709));
#22478=CARTESIAN_POINT('Ctrl Pts',(-149.227912989408,-83.4781527981097,
-46.3072318162821));
#22479=CARTESIAN_POINT('Ctrl Pts',(-149.257371929218,-83.3715229743104,
-46.2786215766946));
#22480=CARTESIAN_POINT('Ctrl Pts',(-149.286670239298,-83.265210223348,-46.2486743918971));
#22481=CARTESIAN_POINT('Ctrl Pts',(-149.30536712493,-83.1973661278873,-46.2295634231207));
#22482=CARTESIAN_POINT('Ctrl Pts',(-149.323998297478,-83.1296521693962,
-46.2099077590292));
#22483=CARTESIAN_POINT('Ctrl Pts',(-149.342561050911,-83.0620783213206,
-46.1896652845064));
#22484=CARTESIAN_POINT('Ctrl Pts',(-149.371267458519,-82.95757860723,-46.1583612688204));
#22485=CARTESIAN_POINT('Ctrl Pts',(-149.399774767598,-82.8535435891935,
-46.1257402426392));
#22486=CARTESIAN_POINT('Ctrl Pts',(-149.428061694081,-82.7500633861384,
-46.0915220141326));
#22487=CARTESIAN_POINT('Ctrl Pts',(-149.454923581065,-82.6517963113774,
-46.0590276324095));
#22488=CARTESIAN_POINT('Ctrl Pts',(-149.48158676368,-82.5540293874111,-46.0250930589968));
#22489=CARTESIAN_POINT('Ctrl Pts',(-149.508023085913,-82.4568752754022,
-45.9894478142867));
#22490=CARTESIAN_POINT('Ctrl Pts',(-149.512553176896,-82.4402270834634,
-45.9833396953057));
#22491=CARTESIAN_POINT('Ctrl Pts',(-149.517076580988,-82.4235969779237,
-45.9771812656855));
#22492=CARTESIAN_POINT('Ctrl Pts',(-149.521593124104,-82.406985643267,-45.9709710636017));
#22493=CARTESIAN_POINT('Ctrl Pts',(-149.546047412515,-82.3170455368253,
-45.9373466590614));
#22494=CARTESIAN_POINT('Ctrl Pts',(-149.570311794236,-82.2276143985462,
-45.9021926455905));
#22495=CARTESIAN_POINT('Ctrl Pts',(-149.594353719118,-82.1388178247614,
-45.8652538583403));
#22496=CARTESIAN_POINT('Ctrl Pts',(-149.612438155897,-82.07202466936,-45.8374683475715));
#22497=CARTESIAN_POINT('Ctrl Pts',(-149.63039654831,-82.0055912015912,-45.8086724394745));
#22498=CARTESIAN_POINT('Ctrl Pts',(-149.648211128679,-81.9395854582945,
-45.7787450670962));
#22499=CARTESIAN_POINT('Ctrl Pts',(-149.655934224025,-81.9109702095313,
-45.7657707536098));
#22500=CARTESIAN_POINT('Ctrl Pts',(-149.663637104736,-81.8824099165123,
-45.7525620980052));
#22501=CARTESIAN_POINT('Ctrl Pts',(-149.67131055004,-81.8539394834478,-45.7391147562166));
#22502=CARTESIAN_POINT('Ctrl Pts',(-149.685698655415,-81.8005559543078,
-45.7139002973917));
#22503=CARTESIAN_POINT('Ctrl Pts',(-149.699999360789,-81.7474243597972,
-45.6878211143421));
#22504=CARTESIAN_POINT('Ctrl Pts',(-149.714175605301,-81.6946906272146,
-45.6607798441796));
#22505=CARTESIAN_POINT('Ctrl Pts',(-149.727286670739,-81.6459192182512,
-45.6357704093948));
#22506=CARTESIAN_POINT('Ctrl Pts',(-149.740291333114,-81.5974878781543,
-45.6099378953754));
#22507=CARTESIAN_POINT('Ctrl Pts',(-149.75314895044,-81.549552803929,-45.583195140044));
#22508=CARTESIAN_POINT('Ctrl Pts',(-149.76292982072,-81.5130882918071,-45.5628517580484));
#22509=CARTESIAN_POINT('Ctrl Pts',(-149.772625404106,-81.4769116545282,
-45.5419814455611));
#22510=CARTESIAN_POINT('Ctrl Pts',(-149.782212501331,-81.4411109947051,
-45.5205420615612));
#22511=CARTESIAN_POINT('Ctrl Pts',(-149.792712453297,-81.4019015030656,
-45.4970612835013));
#22512=CARTESIAN_POINT('Ctrl Pts',(-149.80309231573,-81.3631061432697,-45.4728977376122));
#22513=CARTESIAN_POINT('Ctrl Pts',(-149.813325028167,-81.3248298095044,
-45.4479419883158));
#22514=CARTESIAN_POINT('Ctrl Pts',(-149.822817814989,-81.2893212306204,
-45.4247907848088));
#22515=CARTESIAN_POINT('Ctrl Pts',(-149.832167251568,-81.2543175533045,
-45.4010004533823));
#22516=CARTESIAN_POINT('Ctrl Pts',(-149.841373631764,-81.2198208404939,
-45.3764055282848));
#22517=CARTESIAN_POINT('Ctrl Pts',(-149.850444720927,-81.1858310691553,
-45.352172034365));
#22518=CARTESIAN_POINT('Ctrl Pts',(-149.859377062136,-81.1523329411743,
-45.3271576500975));
#22519=CARTESIAN_POINT('Ctrl Pts',(-149.868158592942,-81.1193744240714,
-45.3011827166068));
#22520=CARTESIAN_POINT('Ctrl Pts',(-149.876313696672,-81.0887669899374,
-45.2770606948705));
#22521=CARTESIAN_POINT('Ctrl Pts',(-149.884338741479,-81.0586248955663,
-45.2521102789363));
#22522=CARTESIAN_POINT('Ctrl Pts',(-149.8922125854,-81.0290296766821,-45.2261677408448));
#22523=CARTESIAN_POINT('Ctrl Pts',(-149.892817407753,-81.0267563461319,
-45.2241749877375));
#22524=CARTESIAN_POINT('Ctrl Pts',(-149.893421331922,-81.0244862651328,
-45.2221763702828));
#22525=CARTESIAN_POINT('Ctrl Pts',(-149.894024345238,-81.0222194822742,
-45.2201718089514));
#22526=CARTESIAN_POINT('Ctrl Pts',(-149.901678691384,-80.9934460867894,
-45.194726920949));
#22527=CARTESIAN_POINT('Ctrl Pts',(-149.909127380051,-80.9654260581732,
-45.1685200129132));
#22528=CARTESIAN_POINT('Ctrl Pts',(-149.916327644768,-80.9383234966228,
-45.1414142231911));
#22529=CARTESIAN_POINT('Ctrl Pts',(-149.922896825408,-80.9135964026004,
-45.1166841839377));
#22530=CARTESIAN_POINT('Ctrl Pts',(-149.929259164437,-80.8896331987158,
-45.0912058787197));
#22531=CARTESIAN_POINT('Ctrl Pts',(-149.935369835439,-80.8666055523403,
-45.0648643182037));
#22532=CARTESIAN_POINT('Ctrl Pts',(-149.935956871689,-80.864393346322,-45.0623337530841));
#22533=CARTESIAN_POINT('Ctrl Pts',(-149.936541575424,-80.8621898122599,
-45.0597952121657));
#22534=CARTESIAN_POINT('Ctrl Pts',(-149.937123900464,-80.8599951269442,
-45.0572485877254));
#22535=CARTESIAN_POINT('Ctrl Pts',(-149.949888621083,-80.8118870379003,
-45.0014258989527));
#22536=CARTESIAN_POINT('Ctrl Pts',(-149.961572072671,-80.7677918263995,
-44.9414473167645));
#22537=CARTESIAN_POINT('Ctrl Pts',(-149.971367310254,-80.7307169524392,
-44.8772845402088));
#22538=CARTESIAN_POINT('Ctrl Pts',(-149.975158206732,-80.7163684480826,
-44.8524526316788));
#22539=CARTESIAN_POINT('Ctrl Pts',(-149.978650998302,-80.7031305919437,
-44.8269091212123));
#22540=CARTESIAN_POINT('Ctrl Pts',(-149.981796037926,-80.6911891223571,
-44.8007713404859));
#22541=CARTESIAN_POINT('Ctrl Pts',(-149.985757876155,-80.6761463323222,
-44.767845313702));
#22542=CARTESIAN_POINT('Ctrl Pts',(-149.989179977686,-80.6631984113658,
-44.7338784466372));
#22543=CARTESIAN_POINT('Ctrl Pts',(-149.991954976262,-80.6527310533633,
-44.6991041970813));
#22544=CARTESIAN_POINT('Ctrl Pts',(-149.993127423005,-80.6483085574693,
-44.6844119532658));
#22545=CARTESIAN_POINT('Ctrl Pts',(-149.994184300917,-80.6443291875704,
-44.669576131169));
#22546=CARTESIAN_POINT('Ctrl Pts',(-149.995117265699,-80.6408234431072,
-44.6546167402297));
#22547=CARTESIAN_POINT('Ctrl Pts',(-149.997168971269,-80.6331138750976,
-44.6217191793725));
#22548=CARTESIAN_POINT('Ctrl Pts',(-149.998622294847,-80.62769656615,-44.5882207958789));
#22549=CARTESIAN_POINT('Ctrl Pts',(-149.999384955835,-80.6248606269888,
-44.5543174102316));
#22550=CARTESIAN_POINT('Ctrl Pts',(-149.999789923498,-80.6233547630872,
-44.5363149490749));
#22551=CARTESIAN_POINT('Ctrl Pts',(-150.,-80.6225774829854,-44.5181985965764));
#22552=CARTESIAN_POINT('Ctrl Pts',(-150.,-80.6225774829854,-44.5));
#22553=CARTESIAN_POINT('Origin',(-147.5,-122.5,-44.5));
#22554=CARTESIAN_POINT('Origin',(0.,0.,-49.5));
#22555=CARTESIAN_POINT('Origin',(-147.5,-89.4427190999916,-49.5));
#22556=CARTESIAN_POINT('Origin',(-177.5,-137.5,-73.9644660940673));
#22557=CARTESIAN_POINT('Origin',(-177.5,-137.5,-73.9644660940673));
#22558=CARTESIAN_POINT('Origin',(-177.5,-137.5,-73.9644660940673));
#22559=CARTESIAN_POINT('Origin',(-177.5,-137.5,-73.9644660940673));
#22560=CARTESIAN_POINT('Origin',(-168.964466094067,-127.5,-82.5));
#22561=CARTESIAN_POINT('Origin',(-168.964466094067,-127.5,-82.5));
#22562=CARTESIAN_POINT('Origin',(-168.964466094067,-127.5,-82.5));
#22563=CARTESIAN_POINT('Origin',(-168.964466094067,-127.5,-82.5));
#22564=CARTESIAN_POINT('Origin',(-147.5,-122.5,-44.5));
#22565=CARTESIAN_POINT('Origin',(-152.5,-122.5,-44.5));
#22566=CARTESIAN_POINT('Ctrl Pts',(-145.36231884058,-88.1464478086873,-49.5));
#22567=CARTESIAN_POINT('Ctrl Pts',(-145.36231884058,-88.1464478086873,-47.));
#22568=CARTESIAN_POINT('Ctrl Pts',(-147.5,-89.4427190999916,-47.));
#22569=CARTESIAN_POINT('Ctrl Pts',(-145.88328041902,-87.2873300001825,-49.4999999990697));
#22570=CARTESIAN_POINT('Ctrl Pts',(-145.793011707092,-87.4361921450511,
-47.2163561992337));
#22571=CARTESIAN_POINT('Ctrl Pts',(-147.764311380887,-88.5709672327986,
-47.));
#22572=CARTESIAN_POINT('Ctrl Pts',(-146.390924783419,-86.432995377738,-49.4182529717019));
#22573=CARTESIAN_POINT('Ctrl Pts',(-146.25636627112,-86.6602829701382,-47.3466184200069));
#22574=CARTESIAN_POINT('Ctrl Pts',(-148.021866250329,-87.7040688391623,
-46.959126485635));
#22575=CARTESIAN_POINT('Ctrl Pts',(-147.13295559207,-85.1594666843921,-49.1735002410464));
#22576=CARTESIAN_POINT('Ctrl Pts',(-146.95625485105,-85.4644664729224,-47.393964945865));
#22577=CARTESIAN_POINT('Ctrl Pts',(-148.398337763665,-86.4118117826985,
-46.8367501206312));
#22578=CARTESIAN_POINT('Ctrl Pts',(-147.377049426154,-84.7363019818542,
-49.0712223542218));
#22579=CARTESIAN_POINT('Ctrl Pts',(-147.185340564392,-85.0695699101127,
-47.3871528892726));
#22580=CARTESIAN_POINT('Ctrl Pts',(-148.522179488132,-85.9824240698147,
-46.7856111768689));
#22581=CARTESIAN_POINT('Ctrl Pts',(-147.858493843555,-83.8933928830767,
-48.8197197604928));
#22582=CARTESIAN_POINT('Ctrl Pts',(-147.640340054158,-84.2776371924664,
-47.3236601563046));
#22583=CARTESIAN_POINT('Ctrl Pts',(-148.766441729588,-85.1271192490123,
-46.6598598804885));
#22584=CARTESIAN_POINT('Ctrl Pts',(-148.095887496716,-83.4735259621086,
-48.670309617217));
#22585=CARTESIAN_POINT('Ctrl Pts',(-147.866955151253,-83.8795640251351,
-47.2682201155608));
#22586=CARTESIAN_POINT('Ctrl Pts',(-148.886884097334,-84.7010778144719,
-46.5851548082849));
#22587=CARTESIAN_POINT('Ctrl Pts',(-148.555727425865,-82.65238822296,-48.3190668315844));
#22588=CARTESIAN_POINT('Ctrl Pts',(-148.307824862021,-83.0977615436487,
-47.1034791582529));
#22589=CARTESIAN_POINT('Ctrl Pts',(-149.120185238387,-83.867864520377,-46.4095334161157));
#22590=CARTESIAN_POINT('Ctrl Pts',(-148.780093861296,-82.2476812683581,
-48.1160600755383));
#22591=CARTESIAN_POINT('Ctrl Pts',(-148.524727773055,-82.7095240936236,
-46.9949635047617));
#22592=CARTESIAN_POINT('Ctrl Pts',(-149.234018208522,-83.457205992854,-46.308030037322));
#22593=CARTESIAN_POINT('Ctrl Pts',(-149.207972890121,-81.4688789012013,
-47.6426010624872));
#22594=CARTESIAN_POINT('Ctrl Pts',(-148.93931728545,-81.9607628458225,-46.713912421055));
#22595=CARTESIAN_POINT('Ctrl Pts',(-149.4511038933,-82.6669506497871,-46.0713005316908));
#22596=CARTESIAN_POINT('Ctrl Pts',(-149.410469407752,-81.0966396786721,
-47.3745618678272));
#22597=CARTESIAN_POINT('Ctrl Pts',(-149.13707735126,-81.6002642788733,-46.5440613352092));
#22598=CARTESIAN_POINT('Ctrl Pts',(-149.553841095111,-82.2892373209608,
-45.9372809330665));
#22599=CARTESIAN_POINT('Ctrl Pts',(-149.689478100498,-80.5797647052593,
-46.8989514695024));
#22600=CARTESIAN_POINT('Ctrl Pts',(-149.410828634125,-81.0973762069276,
-46.2235340082297));
#22601=CARTESIAN_POINT('Ctrl Pts',(-149.695396978193,-81.7647612450649,
-45.6994757351747));
#22602=CARTESIAN_POINT('Ctrl Pts',(-149.778860900691,-80.4134491496535,
-46.7265495064604));
#22603=CARTESIAN_POINT('Ctrl Pts',(-149.498351131341,-80.935915280146,-46.1055106385897));
#22604=CARTESIAN_POINT('Ctrl Pts',(-149.74074560314,-81.5959998724055,-45.6132747528471));
#22605=CARTESIAN_POINT('Ctrl Pts',(-149.942345818684,-80.1081950067706,
-46.3555706163427));
#22606=CARTESIAN_POINT('Ctrl Pts',(-149.658443692203,-80.6395711160542,
-45.8467452989258));
#22607=CARTESIAN_POINT('Ctrl Pts',(-149.823690158896,-81.2862566980837,
-45.4277853085544));
#22608=CARTESIAN_POINT('Ctrl Pts',(-150.016754772459,-79.9686937648418,
-46.1569684467915));
#22609=CARTESIAN_POINT('Ctrl Pts',(-149.731542660712,-80.5037270542566,
-45.7060159661836));
#22610=CARTESIAN_POINT('Ctrl Pts',(-149.861441758745,-81.144703967216,-45.3284842231662));
#22611=CARTESIAN_POINT('Ctrl Pts',(-150.145196691125,-79.7272764209246,
-45.7237173672864));
#22612=CARTESIAN_POINT('Ctrl Pts',(-149.857607243134,-80.2688649285009,
-45.3951674418671));
#22613=CARTESIAN_POINT('Ctrl Pts',(-149.926607145573,-80.8997363683411,
-45.1118586838727));
#22614=CARTESIAN_POINT('Ctrl Pts',(-150.197080555724,-79.6294105444985,
-45.4961190800877));
#22615=CARTESIAN_POINT('Ctrl Pts',(-149.908727602392,-80.1732994372084,
-45.2298837812697));
#22616=CARTESIAN_POINT('Ctrl Pts',(-149.952930574586,-80.8004312877628,
-44.9980595398227));
#22617=CARTESIAN_POINT('Ctrl Pts',(-150.269771338359,-79.4921496315481,
-45.0129350155497));
#22618=CARTESIAN_POINT('Ctrl Pts',(-149.980179574577,-80.0395829024242,
-44.8770900280323));
#22619=CARTESIAN_POINT('Ctrl Pts',(-149.989810459912,-80.6611518320492,
-44.756467507996));
#22620=CARTESIAN_POINT('Ctrl Pts',(-150.289855071895,-79.4541343321333,
-44.7534294495147));
#22621=CARTESIAN_POINT('Ctrl Pts',(-149.99999999943,-80.0024038110911,-44.686188272212));
#22622=CARTESIAN_POINT('Ctrl Pts',(-150.,-80.6225774840775,-44.6267147245865));
#22623=CARTESIAN_POINT('Ctrl Pts',(-150.289855072464,-79.4541343310581,
-44.5));
#22624=CARTESIAN_POINT('Ctrl Pts',(-150.,-80.0024038100394,-44.5));
#22625=CARTESIAN_POINT('Ctrl Pts',(-150.,-80.6225774829855,-44.5));
#22626=CARTESIAN_POINT('Origin',(-152.5,-80.6225774829854,-44.5));
#22627=CARTESIAN_POINT('Origin',(-121.449578014911,-122.5,115.));
#22628=CARTESIAN_POINT('Origin',(-121.449578014911,-122.5,-82.5));
#22629=CARTESIAN_POINT('Origin',(-115.217186218029,-127.5,-82.5));
#22630=CARTESIAN_POINT('Ctrl Pts',(-116.189500386223,-127.5,-85.));
#22631=CARTESIAN_POINT('Ctrl Pts',(-116.448008540164,-127.38221202645,-85.));
#22632=CARTESIAN_POINT('Ctrl Pts',(-116.705458596259,-127.264170864129,
-84.9919054816514));
#22633=CARTESIAN_POINT('Ctrl Pts',(-116.961798715611,-127.145925914751,
-84.9750282599707));
#22634=CARTESIAN_POINT('Ctrl Pts',(-117.203993378032,-127.034206002666,
-84.959082363488));
#22635=CARTESIAN_POINT('Ctrl Pts',(-117.44519709589,-126.922304462312,-84.9352961056291));
#22636=CARTESIAN_POINT('Ctrl Pts',(-117.685352831461,-126.810270252905,
-84.9030396156349));
#22637=CARTESIAN_POINT('Ctrl Pts',(-117.699379204216,-126.803726858975,
-84.901155664992));
#22638=CARTESIAN_POINT('Ctrl Pts',(-117.713401998462,-126.797183013924,
-84.8992428065339));
#22639=CARTESIAN_POINT('Ctrl Pts',(-117.727421201482,-126.790638727993,
-84.8973009093819));
#22640=CARTESIAN_POINT('Ctrl Pts',(-117.801716706967,-126.755956939694,
-84.8870097230497));
#22641=CARTESIAN_POINT('Ctrl Pts',(-117.875811770812,-126.72130622253,-84.8759163529927));
#22642=CARTESIAN_POINT('Ctrl Pts',(-117.949766484241,-126.686659174449,
-84.8639959183808));
#22643=CARTESIAN_POINT('Ctrl Pts',(-118.068035959454,-126.631251100991,
-84.8449325824487));
#22644=CARTESIAN_POINT('Ctrl Pts',(-118.186129688152,-126.575765453047,
-84.8236742085077));
#22645=CARTESIAN_POINT('Ctrl Pts',(-118.304009972751,-126.520223268687,
-84.8000156545));
#22646=CARTESIAN_POINT('Ctrl Pts',(-118.414673338124,-126.468081512646,
-84.7778055350109));
#22647=CARTESIAN_POINT('Ctrl Pts',(-118.525149041405,-126.415889691706,
-84.7534800370882));
#22648=CARTESIAN_POINT('Ctrl Pts',(-118.635381578983,-126.363674712058,
-84.7268318519906));
#22649=CARTESIAN_POINT('Ctrl Pts',(-118.688420413233,-126.338551262016,
-84.7140099692372));
#22650=CARTESIAN_POINT('Ctrl Pts',(-118.741402540235,-126.313422617281,
-84.7006497952816));
#22651=CARTESIAN_POINT('Ctrl Pts',(-118.794319125547,-126.288292874884,
-84.6867249125821));
#22652=CARTESIAN_POINT('Ctrl Pts',(-118.89901828691,-126.238571923717,-84.6591735592185));
#22653=CARTESIAN_POINT('Ctrl Pts',(-119.002876811888,-126.18912499207,-84.6295858023532));
#22654=CARTESIAN_POINT('Ctrl Pts',(-119.105920148863,-126.139946013055,
-84.5977086876026));
#22655=CARTESIAN_POINT('Ctrl Pts',(-119.148229575834,-126.119753204066,
-84.5846199960073));
#22656=CARTESIAN_POINT('Ctrl Pts',(-119.190401214652,-126.099605728962,
-84.5711448947655));
#22657=CARTESIAN_POINT('Ctrl Pts',(-119.232435280194,-126.079503870074,
-84.5572639252337));
#22658=CARTESIAN_POINT('Ctrl Pts',(-119.332253758365,-126.031767898387,
-84.5243007265441));
#22659=CARTESIAN_POINT('Ctrl Pts',(-119.431308801215,-125.984284516973,
-84.4890488616581));
#22660=CARTESIAN_POINT('Ctrl Pts',(-119.529560384293,-125.937075343597,
-84.4512249355449));
#22661=CARTESIAN_POINT('Ctrl Pts',(-119.549179492618,-125.927648504279,
-84.4436721645821));
#22662=CARTESIAN_POINT('Ctrl Pts',(-119.568766466804,-125.918232645452,
-84.4360167122206));
#22663=CARTESIAN_POINT('Ctrl Pts',(-119.588320838716,-125.908828011419,
-84.4282561299978));
#22664=CARTESIAN_POINT('Ctrl Pts',(-119.676176605187,-125.866573965367,
-84.3933886383424));
#22665=CARTESIAN_POINT('Ctrl Pts',(-119.763367641033,-125.824549754932,
-84.3563903280335));
#22666=CARTESIAN_POINT('Ctrl Pts',(-119.849778269352,-125.78281394182,-84.3169432874789));
#22667=CARTESIAN_POINT('Ctrl Pts',(-119.884154184046,-125.766210582034,
-84.3012504482132));
#22668=CARTESIAN_POINT('Ctrl Pts',(-119.918406261835,-125.749653027024,
-84.285169643908));
#22669=CARTESIAN_POINT('Ctrl Pts',(-119.952525858354,-125.73314564101,-84.2686790921246));
#22670=CARTESIAN_POINT('Ctrl Pts',(-119.954356344091,-125.732260034563,
-84.2677943888192));
#22671=CARTESIAN_POINT('Ctrl Pts',(-119.956186462171,-125.731374563089,
-84.2669084964012));
#22672=CARTESIAN_POINT('Ctrl Pts',(-119.95801621397,-125.730489226021,-84.2660214100551));
#22673=CARTESIAN_POINT('Ctrl Pts',(-120.016911873287,-125.701992185948,
-84.2374680645811));
#22674=CARTESIAN_POINT('Ctrl Pts',(-120.075514267379,-125.673592123274,
-84.2076160589801));
#22675=CARTESIAN_POINT('Ctrl Pts',(-120.133520234545,-125.645440552611,
-84.1764738678679));
#22676=CARTESIAN_POINT('Ctrl Pts',(-120.185326529737,-125.620297819008,
-84.1486601510297));
#22677=CARTESIAN_POINT('Ctrl Pts',(-120.236657062529,-125.59535329509,-84.1198170380798));
#22678=CARTESIAN_POINT('Ctrl Pts',(-120.287252932554,-125.570735521226,
-84.0899486389992));
#22679=CARTESIAN_POINT('Ctrl Pts',(-120.293307752653,-125.567789506227,
-84.0863742804003));
#22680=CARTESIAN_POINT('Ctrl Pts',(-120.299351995995,-125.564848197422,
-84.0827852386968));
#22681=CARTESIAN_POINT('Ctrl Pts',(-120.305385171906,-125.561911837745,
-84.079181521328));
#22682=CARTESIAN_POINT('Ctrl Pts',(-120.360569807383,-125.535053357107,
-84.0462188110888));
#22683=CARTESIAN_POINT('Ctrl Pts',(-120.414989618108,-125.50853101205,-84.0119891408405));
#22684=CARTESIAN_POINT('Ctrl Pts',(-120.468555276039,-125.482393019766,
-83.9762964268604));
#22685=CARTESIAN_POINT('Ctrl Pts',(-120.521845432248,-125.456389461785,
-83.9407872895329));
#22686=CARTESIAN_POINT('Ctrl Pts',(-120.574290544884,-125.430766130918,
-83.9038303719348));
#22687=CARTESIAN_POINT('Ctrl Pts',(-120.625763505242,-125.405589684656,
-83.8652058122217));
#22688=CARTESIAN_POINT('Ctrl Pts',(-120.669724343266,-125.384087566487,
-83.8322182396883));
#22689=CARTESIAN_POINT('Ctrl Pts',(-120.712919977839,-125.362939699074,
-83.7980586074073));
#22690=CARTESIAN_POINT('Ctrl Pts',(-120.755308589257,-125.342167431334,
-83.7625256624013));
#22691=CARTESIAN_POINT('Ctrl Pts',(-120.796119057648,-125.322168522485,
-83.7283156215319));
#22692=CARTESIAN_POINT('Ctrl Pts',(-120.836181594647,-125.302517695472,
-83.6928327066298));
#22693=CARTESIAN_POINT('Ctrl Pts',(-120.875421453446,-125.283252598417,
-83.6558720771509));
#22694=CARTESIAN_POINT('Ctrl Pts',(-120.882694505649,-125.279681839988,
-83.6490214768709));
#22695=CARTESIAN_POINT('Ctrl Pts',(-120.889939185328,-125.276124387981,
-83.6421200366566));
#22696=CARTESIAN_POINT('Ctrl Pts',(-120.897154862446,-125.27258055919,-83.6351663481079));
#22697=CARTESIAN_POINT('Ctrl Pts',(-120.930420737934,-125.256242720708,
-83.6031082981616));
#22698=CARTESIAN_POINT('Ctrl Pts',(-120.96296989403,-125.240243618619,-83.5699873691134));
#22699=CARTESIAN_POINT('Ctrl Pts',(-120.994602600046,-125.224682872272,
-83.5357995420531));
#22700=CARTESIAN_POINT('Ctrl Pts',(-121.02464265881,-125.209905580236,-83.5033330077842));
#22701=CARTESIAN_POINT('Ctrl Pts',(-121.053856347371,-125.195523551208,
-83.4699041219391));
#22702=CARTESIAN_POINT('Ctrl Pts',(-121.082031519278,-125.18164267959,-83.4355171689384));
#22703=CARTESIAN_POINT('Ctrl Pts',(-121.097985602238,-125.173782689309,
-83.416045688775));
#22704=CARTESIAN_POINT('Ctrl Pts',(-121.11360593729,-125.166083770046,-83.3962671746067));
#22705=CARTESIAN_POINT('Ctrl Pts',(-121.128847427401,-125.158568448299,
-83.376183935507));
#22706=CARTESIAN_POINT('Ctrl Pts',(-121.149706220237,-125.148283329307,
-83.3486989507179));
#22707=CARTESIAN_POINT('Ctrl Pts',(-121.169911626187,-125.138314491271,
-83.3205937206655));
#22708=CARTESIAN_POINT('Ctrl Pts',(-121.189383694811,-125.128702127376,
-83.2918112814196));
#22709=CARTESIAN_POINT('Ctrl Pts',(-121.219288926774,-125.113939444605,
-83.247607168403));
#22710=CARTESIAN_POINT('Ctrl Pts',(-121.247502565948,-125.100002690926,
-83.2017508061736));
#22711=CARTESIAN_POINT('Ctrl Pts',(-121.273533474804,-125.08713705477,-83.1542957064863));
#22712=CARTESIAN_POINT('Ctrl Pts',(-121.283706281802,-125.082109199836,
-83.135750385119));
#22713=CARTESIAN_POINT('Ctrl Pts',(-121.293546196394,-125.077244718342,
-83.1169610513985));
#22714=CARTESIAN_POINT('Ctrl Pts',(-121.303025858184,-125.072557339689,
-83.0979315436974));
#22715=CARTESIAN_POINT('Ctrl Pts',(-121.323095906427,-125.06263336584,-83.0576428555519));
#22716=CARTESIAN_POINT('Ctrl Pts',(-121.34152898982,-125.053514201558,-83.0161861526794));
#22717=CARTESIAN_POINT('Ctrl Pts',(-121.357996565739,-125.045363893213,
-82.973949637818));
#22718=CARTESIAN_POINT('Ctrl Pts',(-121.365145493274,-125.041825669735,
-82.9556138617733));
#22719=CARTESIAN_POINT('Ctrl Pts',(-121.371924242056,-125.038469923384,
-82.9371317587527));
#22720=CARTESIAN_POINT('Ctrl Pts',(-121.378307256223,-125.035309443556,
-82.9185377169621));
#22721=CARTESIAN_POINT('Ctrl Pts',(-121.391447468896,-125.028803210607,
-82.8802596155573));
#22722=CARTESIAN_POINT('Ctrl Pts',(-121.402999576331,-125.02308111907,-82.841245154545));
#22723=CARTESIAN_POINT('Ctrl Pts',(-121.41267276749,-125.018288884737,-82.8018442319799));
#22724=CARTESIAN_POINT('Ctrl Pts',(-121.42270975789,-125.013316419167,-82.7609614793284));
#22725=CARTESIAN_POINT('Ctrl Pts',(-121.430817047126,-125.009299023436,
-82.7195176677953));
#22726=CARTESIAN_POINT('Ctrl Pts',(-121.436839100795,-125.006314500192,
-82.677630304934));
#22727=CARTESIAN_POINT('Ctrl Pts',(-121.442766130955,-125.003377070495,
-82.6364038933766));
#22728=CARTESIAN_POINT('Ctrl Pts',(-121.446673152346,-125.00144020774,-82.5947478149961));
#22729=CARTESIAN_POINT('Ctrl Pts',(-121.448457146611,-125.00055573514,-82.5527767556245));
#22730=CARTESIAN_POINT('Ctrl Pts',(-121.449202695036,-125.000186105502,
-82.5352366447455));
#22731=CARTESIAN_POINT('Ctrl Pts',(-121.449578014744,-125.,-82.5176415553729));
#22732=CARTESIAN_POINT('Ctrl Pts',(-121.449578014911,-125.,-82.5));
#22733=CARTESIAN_POINT('Origin',(-168.964466094067,0.,-82.5));
#22734=CARTESIAN_POINT('Origin',(-168.964466094067,-137.5,-82.5));
#22735=CARTESIAN_POINT('Origin',(-258.232233047034,-137.5,6.76776695296637));
#22736=CARTESIAN_POINT('Origin',(-168.964466094067,-137.5,-82.5));
#22737=CARTESIAN_POINT('Origin',(-177.5,-137.5,85.));
#22738=CARTESIAN_POINT('Origin',(-177.5,-137.5,73.9644660940671));
#22739=CARTESIAN_POINT('Origin',(-177.5,-125.,-73.9644660940673));
#22740=CARTESIAN_POINT('Origin',(-177.5,-127.5,-73.9644660940673));
#22741=CARTESIAN_POINT('Origin',(-225.840826156048,-127.5,-25.6236399380191));
#22742=CARTESIAN_POINT('Origin',(-177.5,-127.5,-73.9644660940673));
#22743=CARTESIAN_POINT('Origin',(-152.5,-122.5,-47.));
#22744=CARTESIAN_POINT('Origin',(-152.5,-122.5,-37.5));
#22745=CARTESIAN_POINT('Origin',(-147.5,0.,-37.5));
#22746=CARTESIAN_POINT('Ctrl Pts',(-150.,-80.6225774829854,-37.5));
#22747=CARTESIAN_POINT('Ctrl Pts',(-150.,-80.6225774829854,-37.4687656111694));
#22748=CARTESIAN_POINT('Ctrl Pts',(-149.999418286665,-80.6247797743348,
-37.4378789835208));
#22749=CARTESIAN_POINT('Ctrl Pts',(-149.998293554945,-80.6290354954266,
-37.407427664437));
#22750=CARTESIAN_POINT('Ctrl Pts',(-149.997125538082,-80.6334549973543,
-37.3758044305615));
#22751=CARTESIAN_POINT('Ctrl Pts',(-149.995371936956,-80.6400888791783,
-37.3446506435411));
#22752=CARTESIAN_POINT('Ctrl Pts',(-149.993090530187,-80.6487160556982,
-37.3140587875661));
#22753=CARTESIAN_POINT('Ctrl Pts',(-149.992231155702,-80.6519657941863,
-37.3025352570627));
#22754=CARTESIAN_POINT('Ctrl Pts',(-149.991297028852,-80.6554978429528,
-37.2910914065902));
#22755=CARTESIAN_POINT('Ctrl Pts',(-149.990291719683,-80.6592985775913,
-37.2797319931106));
#22756=CARTESIAN_POINT('Ctrl Pts',(-149.987499102739,-80.6698565196466,
-37.2481770331612));
#22757=CARTESIAN_POINT('Ctrl Pts',(-149.984157100677,-80.6824881297729,
-37.2172858271412));
#22758=CARTESIAN_POINT('Ctrl Pts',(-149.980355786964,-80.6968505802923,
-37.1871743733059));
#22759=CARTESIAN_POINT('Ctrl Pts',(-149.977558137322,-80.7074209008703,
-37.1650132720595));
#22760=CARTESIAN_POINT('Ctrl Pts',(-149.974509955706,-80.7189351701335,
-37.1432550493073));
#22761=CARTESIAN_POINT('Ctrl Pts',(-149.971243495187,-80.7312708109916,
-37.1219053194033));
#22762=CARTESIAN_POINT('Ctrl Pts',(-149.965898079906,-80.7514575307658,
-37.0869674495522));
#22763=CARTESIAN_POINT('Ctrl Pts',(-149.960009186175,-80.7736866486582,
-37.0534295032029));
#22764=CARTESIAN_POINT('Ctrl Pts',(-149.953740444396,-80.7973352935883,
-37.0212984263663));
#22765=CARTESIAN_POINT('Ctrl Pts',(-149.948225014273,-80.8181420923422,
-36.9930285254284));
#22766=CARTESIAN_POINT('Ctrl Pts',(-149.942415420697,-80.8400482471093,
-36.9658474797142));
#22767=CARTESIAN_POINT('Ctrl Pts',(-149.936415096464,-80.8626613647233,
-36.9397533647229));
#22768=CARTESIAN_POINT('Ctrl Pts',(-149.930229230798,-80.8859737229203,
-36.9128523700925));
#22769=CARTESIAN_POINT('Ctrl Pts',(-149.923781601043,-80.910257863373,-36.8868469814865));
#22770=CARTESIAN_POINT('Ctrl Pts',(-149.917129634266,-80.9352949903568,
-36.8616578829437));
#22771=CARTESIAN_POINT('Ctrl Pts',(-149.910169623637,-80.9614915538333,
-36.8353023103049));
#22772=CARTESIAN_POINT('Ctrl Pts',(-149.902985851618,-80.9885126935554,
-36.8098403335372));
#22773=CARTESIAN_POINT('Ctrl Pts',(-149.895629953762,-81.0161619977779,
-36.7851874043746));
#22774=CARTESIAN_POINT('Ctrl Pts',(-149.894768894783,-81.0193985410422,
-36.7823016076404));
#22775=CARTESIAN_POINT('Ctrl Pts',(-149.893905462669,-81.0226437476004,
-36.7794269040105));
#22776=CARTESIAN_POINT('Ctrl Pts',(-149.893039728921,-81.0258973457803,
-36.776563163654));
#22777=CARTESIAN_POINT('Ctrl Pts',(-149.885294621978,-81.0550049852878,
-36.7509433060895));
#22778=CARTESIAN_POINT('Ctrl Pts',(-149.877335285321,-81.0848961910516,
-36.7261125791003));
#22779=CARTESIAN_POINT('Ctrl Pts',(-149.869211724908,-81.1153826082327,
-36.7020057411971));
#22780=CARTESIAN_POINT('Ctrl Pts',(-149.860756318488,-81.1471143901678,
-36.6769141432259));
#22781=CARTESIAN_POINT('Ctrl Pts',(-149.852122886993,-81.1794914281188,
-36.652606677046));
#22782=CARTESIAN_POINT('Ctrl Pts',(-149.843353240434,-81.2123567796228,
-36.6290138576759));
#22783=CARTESIAN_POINT('Ctrl Pts',(-149.83403385977,-81.2472823286997,-36.603942098724));
#22784=CARTESIAN_POINT('Ctrl Pts',(-149.824560562648,-81.2827596738303,
-36.5796772330309));
#22785=CARTESIAN_POINT('Ctrl Pts',(-149.814968902627,-81.3186560160361,
-36.5561425173624));
#22786=CARTESIAN_POINT('Ctrl Pts',(-149.814245534129,-81.3213631890505,
-36.5543676137582));
#22787=CARTESIAN_POINT('Ctrl Pts',(-149.813521486333,-81.3240727682797,
-36.5525968666158));
#22788=CARTESIAN_POINT('Ctrl Pts',(-149.812796771609,-81.3267847076915,
-36.550830244838));
#22789=CARTESIAN_POINT('Ctrl Pts',(-149.802161746897,-81.3665818053883,
-36.5249054696828));
#22790=CARTESIAN_POINT('Ctrl Pts',(-149.791378236576,-81.4068954418299,
-36.4998550500824));
#22791=CARTESIAN_POINT('Ctrl Pts',(-149.780505488345,-81.4474999785173,
-36.4756491236568));
#22792=CARTESIAN_POINT('Ctrl Pts',(-149.766212096435,-81.5008789903243,
-36.4438278411627));
#22793=CARTESIAN_POINT('Ctrl Pts',(-149.751731044149,-81.5548874755392,
-36.4133414348064));
#22794=CARTESIAN_POINT('Ctrl Pts',(-149.737090172798,-81.6094178533142,
-36.3839845210638));
#22795=CARTESIAN_POINT('Ctrl Pts',(-149.721679195216,-81.6668165155451,
-36.3530834408805));
#22796=CARTESIAN_POINT('Ctrl Pts',(-149.706091100879,-81.7247936014414,
-36.3234339148103));
#22797=CARTESIAN_POINT('Ctrl Pts',(-149.69034564287,-81.7832715017069,-36.2948268672517));
#22798=CARTESIAN_POINT('Ctrl Pts',(-149.684002656686,-81.8068290580035,
-36.2833026481829));
#22799=CARTESIAN_POINT('Ctrl Pts',(-149.677633997879,-81.8304683944444,
-36.2719479292499));
#22800=CARTESIAN_POINT('Ctrl Pts',(-149.671240444102,-81.8541863565932,
-36.2607502650746));
#22801=CARTESIAN_POINT('Ctrl Pts',(-149.663115656512,-81.8843266214972,
-36.2465205196002));
#22802=CARTESIAN_POINT('Ctrl Pts',(-149.654955183208,-81.9145791058626,
-36.2325522508595));
#22803=CARTESIAN_POINT('Ctrl Pts',(-149.646761444289,-81.9449339838539,
-36.2188226892616));
#22804=CARTESIAN_POINT('Ctrl Pts',(-149.629599044992,-82.0085145472293,
-36.1900650951265));
#22805=CARTESIAN_POINT('Ctrl Pts',(-149.612256027534,-82.0726719053156,
-36.1623178493706));
#22806=CARTESIAN_POINT('Ctrl Pts',(-149.594776281631,-82.1372383448625,
-36.1354843277007));
#22807=CARTESIAN_POINT('Ctrl Pts',(-149.575926055091,-82.2068670465097,
-36.1065469526865));
#22808=CARTESIAN_POINT('Ctrl Pts',(-149.556916727561,-82.2769718986875,
-36.0786720183562));
#22809=CARTESIAN_POINT('Ctrl Pts',(-149.537787182936,-82.3473991049003,
-36.0517539381258));
#22810=CARTESIAN_POINT('Ctrl Pts',(-149.532245072395,-82.3678029027717,
-36.0439553742236));
#22811=CARTESIAN_POINT('Ctrl Pts',(-149.52669278014,-82.3882340721045,-36.0362372267143));
#22812=CARTESIAN_POINT('Ctrl Pts',(-149.521131044556,-82.4086895813365,
-36.0285971804472));
#22813=CARTESIAN_POINT('Ctrl Pts',(-149.513307047731,-82.4374654619681,
-36.0178495106185));
#22814=CARTESIAN_POINT('Ctrl Pts',(-149.505462657807,-82.4662967316409,
-36.007254069327));
#22815=CARTESIAN_POINT('Ctrl Pts',(-149.497602582525,-82.4951656238998,
-35.9968087539204));
#22816=CARTESIAN_POINT('Ctrl Pts',(-149.466886299756,-82.6079819807508,
-35.955989645942));
#22817=CARTESIAN_POINT('Ctrl Pts',(-149.435949796466,-82.7213062383942,
-35.9174537341956));
#22818=CARTESIAN_POINT('Ctrl Pts',(-149.404819096582,-82.8350358340491,
-35.8808341284359));
#22819=CARTESIAN_POINT('Ctrl Pts',(-149.382928718802,-82.9150078174297,
-35.855084080822));
#22820=CARTESIAN_POINT('Ctrl Pts',(-149.360942099018,-82.9951810078626,
-35.8302825444958));
#22821=CARTESIAN_POINT('Ctrl Pts',(-149.338865605393,-83.0755291035975,
-35.8063136992629));
#22822=CARTESIAN_POINT('Ctrl Pts',(-149.302572702508,-83.2076182697917,
-35.7669098434218));
#22823=CARTESIAN_POINT('Ctrl Pts',(-149.266041574135,-83.340162369254,-35.7297345827364));
#22824=CARTESIAN_POINT('Ctrl Pts',(-149.229255373732,-83.4732146574342,
-35.6944829487595));
#22825=CARTESIAN_POINT('Ctrl Pts',(-149.222100057111,-83.4990947765716,
-35.6876261220217));
#22826=CARTESIAN_POINT('Ctrl Pts',(-149.214935059984,-83.5249942184477,
-35.6808421975269));
#22827=CARTESIAN_POINT('Ctrl Pts',(-149.207760216038,-83.550913508967,-35.674129103287));
#22828=CARTESIAN_POINT('Ctrl Pts',(-149.164019348341,-83.7089284101932,
-35.6332032560904));
#22829=CARTESIAN_POINT('Ctrl Pts',(-149.119950314828,-83.8675446159095,
-35.5949411222395));
#22830=CARTESIAN_POINT('Ctrl Pts',(-149.075578120357,-84.0266555942609,
-35.5589506769715));
#22831=CARTESIAN_POINT('Ctrl Pts',(-149.05085132556,-84.1153215833694,-35.5388946854792));
#22832=CARTESIAN_POINT('Ctrl Pts',(-149.026030206994,-84.2041418314535,
-35.5195449132868));
#22833=CARTESIAN_POINT('Ctrl Pts',(-149.001117827171,-84.2931021083258,
-35.5008388586839));
#22834=CARTESIAN_POINT('Ctrl Pts',(-148.961812515426,-84.4334584869733,
-35.4713255278453));
#22835=CARTESIAN_POINT('Ctrl Pts',(-148.922228706232,-84.5743409203764,
-35.4434175359833));
#22836=CARTESIAN_POINT('Ctrl Pts',(-148.882458149794,-84.7154243069166,
-35.4170237357497));
#22837=CARTESIAN_POINT('Ctrl Pts',(-148.823378479995,-84.9250054804708,
-35.3778154082267));
#22838=CARTESIAN_POINT('Ctrl Pts',(-148.763691428328,-85.1357176967391,
-35.3418193924504));
#22839=CARTESIAN_POINT('Ctrl Pts',(-148.703725142255,-85.3463732564986,
-35.3088731061832));
#22840=CARTESIAN_POINT('Ctrl Pts',(-148.683093735184,-85.4188493241311,
-35.2975379329057));
#22841=CARTESIAN_POINT('Ctrl Pts',(-148.662429146897,-85.4913191023785,
-35.2865639616344));
#22842=CARTESIAN_POINT('Ctrl Pts',(-148.64174438629,-85.5637353575988,-35.2759451993142));
#22843=CARTESIAN_POINT('Ctrl Pts',(-148.565624143803,-85.8302283092078,
-35.2368679879267));
#22844=CARTESIAN_POINT('Ctrl Pts',(-148.489028564946,-86.0967324998969,
-35.2024345741108));
#22845=CARTESIAN_POINT('Ctrl Pts',(-148.411875341856,-86.363523818803,-35.1722187734026));
#22846=CARTESIAN_POINT('Ctrl Pts',(-148.365096720872,-86.5252815456893,
-35.1538986899057));
#22847=CARTESIAN_POINT('Ctrl Pts',(-148.318112977961,-86.6871449973961,
-35.137130141918));
#22848=CARTESIAN_POINT('Ctrl Pts',(-148.270904619886,-86.8491769961468,
-35.1218271577707));
#22849=CARTESIAN_POINT('Ctrl Pts',(-148.249186544881,-86.9237193705388,
-35.1147870620957));
#22850=CARTESIAN_POINT('Ctrl Pts',(-148.227421070419,-86.9982969676296,
-35.1080522041554));
#22851=CARTESIAN_POINT('Ctrl Pts',(-148.205605817643,-87.0729174681583,
-35.1016219420906));
#22852=CARTESIAN_POINT('Ctrl Pts',(-148.101900684581,-87.4276476661539,
-35.0710538258322));
#22853=CARTESIAN_POINT('Ctrl Pts',(-147.997167488998,-87.7829762377465,
-35.0474026555606));
#22854=CARTESIAN_POINT('Ctrl Pts',(-147.891499227655,-88.138532391371,-35.0306489702423));
#22855=CARTESIAN_POINT('Ctrl Pts',(-147.78574533598,-88.4943766768485,-35.0138817082488));
#22856=CARTESIAN_POINT('Ctrl Pts',(-147.679054864753,-88.8504488623489,
-35.0040231183754));
#22857=CARTESIAN_POINT('Ctrl Pts',(-147.571529966672,-89.2063722165035,
-35.0010024709468));
#22858=CARTESIAN_POINT('Ctrl Pts',(-147.547727112024,-89.2851631943715,
-35.0003337883163));
#22859=CARTESIAN_POINT('Ctrl Pts',(-147.523883400841,-89.3639468609495,
-35.));
#22860=CARTESIAN_POINT('Ctrl Pts',(-147.5,-89.4427190999916,-35.));
#22861=CARTESIAN_POINT('Origin',(-147.5,-122.5,-37.5));
#22862=CARTESIAN_POINT('Origin',(-152.5,-80.6225774829854,115.));
#22863=CARTESIAN_POINT('Origin',(-152.5,-80.6225774829854,-37.5));
#22864=CARTESIAN_POINT('Ctrl Pts',(-114.505594583524,-125.652173913043,
-87.5));
#22865=CARTESIAN_POINT('Ctrl Pts',(-114.505594583524,-125.652173913043,
-85.));
#22866=CARTESIAN_POINT('Ctrl Pts',(-116.189500386223,-127.5,-85.));
#22867=CARTESIAN_POINT('Ctrl Pts',(-115.098666513068,-125.111713276284,
-87.4999999993277));
#22868=CARTESIAN_POINT('Ctrl Pts',(-114.980468455819,-125.21942600709,-84.7891971375595));
#22869=CARTESIAN_POINT('Ctrl Pts',(-116.791295074217,-127.225795199449,
-85.));
#22870=CARTESIAN_POINT('Ctrl Pts',(-115.677248330335,-124.576762485167,
-87.412213589489));
#22871=CARTESIAN_POINT('Ctrl Pts',(-115.390477170765,-124.841163526192,
-84.4869181320101));
#22872=CARTESIAN_POINT('Ctrl Pts',(-117.378384335172,-126.95438684932,-84.9561067940532));
#22873=CARTESIAN_POINT('Ctrl Pts',(-116.521921487208,-123.785260415244,
-87.135895140949));
#22874=CARTESIAN_POINT('Ctrl Pts',(-115.879476439131,-124.389591527247,
-83.9347335464694));
#22875=CARTESIAN_POINT('Ctrl Pts',(-118.235479156148,-126.552815945855,
-84.8179475708202));
#22876=CARTESIAN_POINT('Ctrl Pts',(-116.800657852351,-123.522253316272,
-87.0187226097842));
#22877=CARTESIAN_POINT('Ctrl Pts',(-116.025791458685,-124.254393807365,
-83.7225655755117));
#22878=CARTESIAN_POINT('Ctrl Pts',(-118.518314585434,-126.419378520878,
-84.759361304629));
#22879=CARTESIAN_POINT('Ctrl Pts',(-117.34468969422,-123.005546784032,-86.7281977784604));
#22880=CARTESIAN_POINT('Ctrl Pts',(-116.260513692639,-124.039299071365,
-83.2680355386611));
#22881=CARTESIAN_POINT('Ctrl Pts',(-119.070346895646,-126.157225941776,
-84.6140988894933));
#22882=CARTESIAN_POINT('Ctrl Pts',(-117.60597211412,-122.755671483611,-86.5572347078813));
#22883=CARTESIAN_POINT('Ctrl Pts',(-116.343854196174,-123.964200078234,
-83.0270891162966));
#22884=CARTESIAN_POINT('Ctrl Pts',(-119.335471703986,-126.03045097373,-84.5286173533875));
#22885=CARTESIAN_POINT('Ctrl Pts',(-117.979759695142,-122.396103662868,
-86.2561620132639));
#22886=CARTESIAN_POINT('Ctrl Pts',(-116.408893575194,-123.910132089278,
-82.6723188019287));
#22887=CARTESIAN_POINT('Ctrl Pts',(-119.714756161271,-125.848023181682,
-84.3780810069086));
#22888=CARTESIAN_POINT('Ctrl Pts',(-118.101314578112,-122.278806587616,
-86.1483179654515));
#22889=CARTESIAN_POINT('Ctrl Pts',(-116.420127652016,-123.902387828605,
-82.5524859464439));
#22890=CARTESIAN_POINT('Ctrl Pts',(-119.838098616001,-125.788512166127,
-84.3241589823631));
#22891=CARTESIAN_POINT('Ctrl Pts',(-118.337674566633,-122.050079163151,
-85.9157683721022));
#22892=CARTESIAN_POINT('Ctrl Pts',(-116.419552940988,-123.909688381786,
-82.3194835992922));
#22893=CARTESIAN_POINT('Ctrl Pts',(-120.077934486754,-125.672466633894,
-84.2078841864137));
#22894=CARTESIAN_POINT('Ctrl Pts',(-118.452813811182,-121.938320691335,
-85.7905474845089));
#22895=CARTESIAN_POINT('Ctrl Pts',(-116.406751222323,-123.925725220726,
-82.2063383456552));
#22896=CARTESIAN_POINT('Ctrl Pts',(-120.194766955425,-125.615765645109,
-84.1452737420412));
#22897=CARTESIAN_POINT('Ctrl Pts',(-118.779955786455,-121.619960181732,
-85.3940930246681));
#22898=CARTESIAN_POINT('Ctrl Pts',(-116.330634260069,-124.011396018774,
-81.8918489994245));
#22899=CARTESIAN_POINT('Ctrl Pts',(-120.526719842218,-125.454244503486,
-83.9470465127606));
#22900=CARTESIAN_POINT('Ctrl Pts',(-118.976188771633,-121.427849190968,
-85.1007432598167));
#22901=CARTESIAN_POINT('Ctrl Pts',(-116.226334686115,-124.121594328844,
-81.7284336163539));
#22902=CARTESIAN_POINT('Ctrl Pts',(-120.725838606432,-125.356776429138,
-83.8003716291909));
#22903=CARTESIAN_POINT('Ctrl Pts',(-119.229508592988,-121.178951530852,
-84.6051856591968));
#22904=CARTESIAN_POINT('Ctrl Pts',(-116.018327623084,-124.338324238805,
-81.6176595477855));
#22905=CARTESIAN_POINT('Ctrl Pts',(-120.982883719394,-125.230497467175,
-83.5525928299572));
#22906=CARTESIAN_POINT('Ctrl Pts',(-119.306430749595,-121.103197399823,
-84.4313845009826));
#22907=CARTESIAN_POINT('Ctrl Pts',(-115.938944698971,-124.420612015484,
-81.6055951047004));
#22908=CARTESIAN_POINT('Ctrl Pts',(-121.060937084107,-125.192063387035,
-83.4656922503483));
#22909=CARTESIAN_POINT('Ctrl Pts',(-119.440303841191,-120.971164568224,
-84.0733653040093));
#22910=CARTESIAN_POINT('Ctrl Pts',(-115.778652442949,-124.586368326783,
-81.6400246699534));
#22911=CARTESIAN_POINT('Ctrl Pts',(-121.196778897721,-125.125076140871,
-83.2866826521477));
#22912=CARTESIAN_POINT('Ctrl Pts',(-119.497839395063,-120.914311737671,
-83.8880856770369));
#22913=CARTESIAN_POINT('Ctrl Pts',(-115.697759349005,-124.669813047921,
-81.6878272780908));
#22914=CARTESIAN_POINT('Ctrl Pts',(-121.255160562605,-125.096231691082,
-83.1940428383556));
#22915=CARTESIAN_POINT('Ctrl Pts',(-119.592195409221,-120.82098824412,-83.5036466079758));
#22916=CARTESIAN_POINT('Ctrl Pts',(-115.551887637618,-124.820142027729,
-81.8435231238005));
#22917=CARTESIAN_POINT('Ctrl Pts',(-121.350904165271,-125.048883740856,
-83.0018233041507));
#22918=CARTESIAN_POINT('Ctrl Pts',(-119.628897626029,-120.784634828299,
-83.3034927483059));
#22919=CARTESIAN_POINT('Ctrl Pts',(-115.488159523427,-124.885734117082,
-81.9531151909483));
#22920=CARTESIAN_POINT('Ctrl Pts',(-121.388146120508,-125.030439729044,
-82.9017463741539));
#22921=CARTESIAN_POINT('Ctrl Pts',(-119.677240002648,-120.736735847766,
-82.9038841796134));
#22922=CARTESIAN_POINT('Ctrl Pts',(-115.400689666882,-124.975740417795,
-82.2081803578402));
#22923=CARTESIAN_POINT('Ctrl Pts',(-121.437199414473,-125.006138040429,
-82.7019420898058));
#22924=CARTESIAN_POINT('Ctrl Pts',(-119.689439202156,-120.724637682096,
-82.7026620014977));
#22925=CARTESIAN_POINT('Ctrl Pts',(-115.377099115996,-124.999999998111,
-82.3529550603246));
#22926=CARTESIAN_POINT('Ctrl Pts',(-121.449578013952,-125.,-82.6013310007496));
#22927=CARTESIAN_POINT('Ctrl Pts',(-119.689439203101,-120.724637681159,
-82.5));
#22928=CARTESIAN_POINT('Ctrl Pts',(-115.377099114166,-125.,-82.5));
#22929=CARTESIAN_POINT('Ctrl Pts',(-121.449578014911,-125.,-82.5));
#22930=CARTESIAN_POINT('Origin',(-116.189500386223,-127.5,-87.5));
#22931=CARTESIAN_POINT('Origin',(-168.964466094067,-137.5,-82.5));
#22932=CARTESIAN_POINT('Origin',(-168.964466094067,-137.5,-82.5));
#22933=CARTESIAN_POINT('Origin',(-177.5,-137.5,73.9644660940671));
#22934=CARTESIAN_POINT('Origin',(-177.5,-137.5,73.9644660940671));
#22935=CARTESIAN_POINT('Origin',(-177.5,-137.5,73.9644660940671));
#22936=CARTESIAN_POINT('Origin',(-177.5,-127.5,-73.9644660940673));
#22937=CARTESIAN_POINT('Origin',(-177.5,-127.5,-73.9644660940673));
#22938=CARTESIAN_POINT('Origin',(-147.5,-122.5,-37.5));
#22939=CARTESIAN_POINT('Origin',(-147.5,-122.5,-32.5));
#22940=CARTESIAN_POINT('Ctrl Pts',(-150.289855072464,-79.4541343310581,
-37.5));
#22941=CARTESIAN_POINT('Ctrl Pts',(-150.,-80.0024038100394,-37.5));
#22942=CARTESIAN_POINT('Ctrl Pts',(-150.,-80.6225774829855,-37.5));
#22943=CARTESIAN_POINT('Ctrl Pts',(-150.28985506853,-79.4541343384987,-37.2405761439445));
#22944=CARTESIAN_POINT('Ctrl Pts',(-149.999999996126,-80.0024038172978,
-37.3094148175651));
#22945=CARTESIAN_POINT('Ctrl Pts',(-150.,-80.6225774905387,-37.370288072025));
#22946=CARTESIAN_POINT('Ctrl Pts',(-150.2701197497,-79.4914922605523,-36.9888304197613));
#22947=CARTESIAN_POINT('Ctrl Pts',(-149.980519833119,-80.0389466368894,
-37.1241843229246));
#22948=CARTESIAN_POINT('Ctrl Pts',(-149.989987226484,-80.6604847938369,
-37.2444152098049));
#22949=CARTESIAN_POINT('Ctrl Pts',(-150.196231486306,-79.6310132970244,
-36.4987912993743));
#22950=CARTESIAN_POINT('Ctrl Pts',(-149.907890955038,-80.1748646486506,
-36.7663952057919));
#22951=CARTESIAN_POINT('Ctrl Pts',(-149.952499797667,-80.8020576101747,
-36.9993956497629));
#22952=CARTESIAN_POINT('Ctrl Pts',(-150.143050717943,-79.7313168859254,
-36.2679996568602));
#22953=CARTESIAN_POINT('Ctrl Pts',(-149.855501091412,-80.2727952833135,
-36.5988602080128));
#22954=CARTESIAN_POINT('Ctrl Pts',(-149.925518380098,-80.9038362519413,
-36.8839998280985));
#22955=CARTESIAN_POINT('Ctrl Pts',(-150.015028469708,-79.9719313539898,
-35.8382849920608));
#22956=CARTESIAN_POINT('Ctrl Pts',(-149.729850869406,-80.5068721381906,
-36.2906206071997));
#22957=CARTESIAN_POINT('Ctrl Pts',(-149.860565913637,-81.1479891679726,
-36.6691424963621));
#22958=CARTESIAN_POINT('Ctrl Pts',(-149.939105635844,-80.1142600764824,
-35.6362636343074));
#22959=CARTESIAN_POINT('Ctrl Pts',(-149.655266820466,-80.6454659181997,
-36.1475015807484));
#22960=CARTESIAN_POINT('Ctrl Pts',(-149.8220462428,-81.2924109599891,-36.5681318166794));
#22961=CARTESIAN_POINT('Ctrl Pts',(-149.775363670976,-80.4199633406166,
-35.2663619775736));
#22962=CARTESIAN_POINT('Ctrl Pts',(-149.494928348598,-80.9422362487731,
-35.8896065722342));
#22963=CARTESIAN_POINT('Ctrl Pts',(-149.738971273161,-81.6026098603025,
-36.3831809892611));
#22964=CARTESIAN_POINT('Ctrl Pts',(-149.686995608736,-80.5843780010491,
-35.096414733337));
#22965=CARTESIAN_POINT('Ctrl Pts',(-149.408398325687,-81.1018541496878,
-35.7733074247595));
#22966=CARTESIAN_POINT('Ctrl Pts',(-149.694137478568,-81.7694423834459,
-36.2982073663223));
#22967=CARTESIAN_POINT('Ctrl Pts',(-149.500255462679,-80.9302925286903,
-34.7789058669457));
#22968=CARTESIAN_POINT('Ctrl Pts',(-149.226078269656,-81.4367533718067,
-35.5604730905987));
#22969=CARTESIAN_POINT('Ctrl Pts',(-149.599394315017,-82.1204438893779,
-36.1394529338191));
#22970=CARTESIAN_POINT('Ctrl Pts',(-149.401347886677,-81.1127763961017,
-34.6307892928536));
#22971=CARTESIAN_POINT('Ctrl Pts',(-149.129574349821,-81.6133256610706,
-35.4636764520014));
#22972=CARTESIAN_POINT('Ctrl Pts',(-149.549213266549,-82.3056113431205,
-36.0653946460516));
#22973=CARTESIAN_POINT('Ctrl Pts',(-149.197899201606,-81.4863922312639,
-34.3564485886733));
#22974=CARTESIAN_POINT('Ctrl Pts',(-148.93165319989,-81.9738530462027,-35.2892543852097));
#22975=CARTESIAN_POINT('Ctrl Pts',(-149.445992976771,-82.6847215287652,
-35.9282242947119));
#22976=CARTESIAN_POINT('Ctrl Pts',(-149.093462145135,-81.6773447374821,
-34.2301909539054));
#22977=CARTESIAN_POINT('Ctrl Pts',(-148.830186520417,-82.1578926315274,
-35.2116962088616));
#22978=CARTESIAN_POINT('Ctrl Pts',(-149.393006529828,-82.8784821601051,
-35.8650954766799));
#22979=CARTESIAN_POINT('Ctrl Pts',(-148.773324875584,-82.2599185303359,
-33.8775006940139));
#22980=CARTESIAN_POINT('Ctrl Pts',(-148.518202139789,-82.721231742148,-35.0014947689296));
#22981=CARTESIAN_POINT('Ctrl Pts',(-149.230583943609,-83.4696232145796,
-35.6887503475526));
#22982=CARTESIAN_POINT('Ctrl Pts',(-148.550873607934,-82.6611103319686,
-33.6767887272455));
#22983=CARTESIAN_POINT('Ctrl Pts',(-148.30315471628,-83.1060920248233,-34.8943924369622));
#22984=CARTESIAN_POINT('Ctrl Pts',(-149.117722639557,-83.8767148956916,
-35.5883943633349));
#22985=CARTESIAN_POINT('Ctrl Pts',(-148.091214058597,-83.4818155627025,
-33.3265667074903));
#22986=CARTESIAN_POINT('Ctrl Pts',(-147.862495369544,-83.8874214153555,
-34.7305155227995));
#22987=CARTESIAN_POINT('Ctrl Pts',(-148.884513014786,-84.7094893209599,
-35.413283354033));
#22988=CARTESIAN_POINT('Ctrl Pts',(-147.853104568993,-83.9028862659571,
-33.1771134341839));
#22989=CARTESIAN_POINT('Ctrl Pts',(-147.635229789707,-84.286581928446,-34.6752930801302));
#22990=CARTESIAN_POINT('Ctrl Pts',(-148.763707465277,-85.1367522404598,
-35.338556716844));
#22991=CARTESIAN_POINT('Ctrl Pts',(-147.372342666232,-84.7444834282116,
-32.9266778278956));
#22992=CARTESIAN_POINT('Ctrl Pts',(-147.180928816256,-85.0771956930355,
-34.6125828689692));
#22993=CARTESIAN_POINT('Ctrl Pts',(-148.519791499653,-85.9907258315643,
-35.2133389141958));
#22994=CARTESIAN_POINT('Ctrl Pts',(-147.128665473948,-85.1668726405084,
-32.8248617968328));
#22995=CARTESIAN_POINT('Ctrl Pts',(-146.952267516985,-85.4713149459695,
-34.6060731019583));
#22996=CARTESIAN_POINT('Ctrl Pts',(-148.396161159612,-86.4193266499308,
-35.162430898305));
#22997=CARTESIAN_POINT('Ctrl Pts',(-146.388097896074,-86.4377602232233,
-32.58126559787));
#22998=CARTESIAN_POINT('Ctrl Pts',(-146.253862108749,-86.6644852388408,
-34.6540449090446));
#22999=CARTESIAN_POINT('Ctrl Pts',(-148.020432020732,-87.7089037559116,
-35.0406327991578));
#23000=CARTESIAN_POINT('Ctrl Pts',(-145.881711078453,-87.2899179999201,
-32.5000000009063));
#23001=CARTESIAN_POINT('Ctrl Pts',(-145.791767290395,-87.4382443129623,
-34.7842689266316));
#23002=CARTESIAN_POINT('Ctrl Pts',(-147.763515165392,-88.5735933110244,
-35.));
#23003=CARTESIAN_POINT('Ctrl Pts',(-145.36231884058,-88.1464478086875,-32.5));
#23004=CARTESIAN_POINT('Ctrl Pts',(-145.36231884058,-88.1464478086874,-35.0000000000001));
#23005=CARTESIAN_POINT('Ctrl Pts',(-147.5,-89.4427190999917,-35.));
#23006=CARTESIAN_POINT('Origin',(-147.5,-89.4427190999916,-32.5));
#23007=CARTESIAN_POINT('Origin',(0.,0.,-87.5));
#23008=CARTESIAN_POINT('Origin',(-104.163333279998,-137.5,-87.5));
#23009=CARTESIAN_POINT('Origin',(-180.,-137.5,-82.5));
#23010=CARTESIAN_POINT('Ctrl Pts',(-97.2111104761179,-140.,-82.5));
#23011=CARTESIAN_POINT('Ctrl Pts',(-97.2111104761179,-140.,-82.6755496768535));
#23012=CARTESIAN_POINT('Ctrl Pts',(-97.2669993053863,-139.980948398877,
-82.8433669193193));
#23013=CARTESIAN_POINT('Ctrl Pts',(-97.4416750152787,-139.921239210978,
-83.1407858319268));
#23014=CARTESIAN_POINT('Ctrl Pts',(-97.5528693408584,-139.883166869044,
-83.2647663586162));
#23015=CARTESIAN_POINT('Ctrl Pts',(-97.7975572341499,-139.799120034918,
-83.4891405228875));
#23016=CARTESIAN_POINT('Ctrl Pts',(-97.9325262666959,-139.752638285023,
-83.5889920461804));
#23017=CARTESIAN_POINT('Ctrl Pts',(-98.2091898573101,-139.657040028271,
-83.7678569462811));
#23018=CARTESIAN_POINT('Ctrl Pts',(-98.3521285688953,-139.607498613007,
-83.8477491623104));
#23019=CARTESIAN_POINT('Ctrl Pts',(-98.7901601853574,-139.455163852716,
-84.0681986935236));
#23020=CARTESIAN_POINT('Ctrl Pts',(-99.0953089605356,-139.348355708036,
-84.1900813067333));
#23021=CARTESIAN_POINT('Ctrl Pts',(-99.7103269532128,-139.131535702876,
-84.4002328533732));
#23022=CARTESIAN_POINT('Ctrl Pts',(-100.021642419245,-139.021028910904,
-84.4887015138217));
#23023=CARTESIAN_POINT('Ctrl Pts',(-100.963515042103,-138.68428076857,-84.7184070178217));
#23024=CARTESIAN_POINT('Ctrl Pts',(-101.60311676071,-138.452377890846,-84.8244784333066));
#23025=CARTESIAN_POINT('Ctrl Pts',(-102.880937057798,-137.982203598024,
-84.96529984463));
#23026=CARTESIAN_POINT('Ctrl Pts',(-103.521414707761,-137.743143193377,
-85.));
#23027=CARTESIAN_POINT('Ctrl Pts',(-104.163333279998,-137.5,-85.));
#23028=CARTESIAN_POINT('Origin',(-173.232233047034,-137.5,78.2322330470336));
#23029=CARTESIAN_POINT('Origin',(-168.964466094067,-137.5,82.5));
#23030=CARTESIAN_POINT('Origin',(-177.5,-125.,73.9644660940671));
#23031=CARTESIAN_POINT('Origin',(-177.5,-127.5,73.9644660940671));
#23032=CARTESIAN_POINT('Origin',(-177.5,-127.5,85.));
#23033=CARTESIAN_POINT('Origin',(-177.5,-127.5,73.9644660940672));
#23034=CARTESIAN_POINT('Origin',(-115.217186218029,-122.5,-32.5));
#23035=CARTESIAN_POINT('Origin',(0.,0.,-32.5));
#23036=CARTESIAN_POINT('Ctrl Pts',(-95.8063843937653,-140.431966711357,
-82.3302220946716));
#23037=CARTESIAN_POINT('Ctrl Pts',(-96.4436693342527,-139.997193891514,
-82.3767164474312));
#23038=CARTESIAN_POINT('Ctrl Pts',(-97.2155465823483,-139.998571769581,
-82.4151232270209));
#23039=CARTESIAN_POINT('Ctrl Pts',(-95.7923535903209,-140.44153068871,-82.6189757789389));
#23040=CARTESIAN_POINT('Ctrl Pts',(-96.4301984592198,-140.006470158917,
-82.5862803340843));
#23041=CARTESIAN_POINT('Ctrl Pts',(-97.2013093103816,-140.003422681504,
-82.5594793863893));
#23042=CARTESIAN_POINT('Ctrl Pts',(-95.8143433314505,-140.426549686738,
-82.8999538047632));
#23043=CARTESIAN_POINT('Ctrl Pts',(-96.4513705556942,-139.991898168234,
-82.7909496905929));
#23044=CARTESIAN_POINT('Ctrl Pts',(-97.2236226187953,-139.995824235922,
-82.6999480513205));
#23045=CARTESIAN_POINT('Ctrl Pts',(-95.9113524568369,-140.360304954438,
-83.3940569629634));
#23046=CARTESIAN_POINT('Ctrl Pts',(-96.5440906351143,-139.927939556875,
-83.1478648493756));
#23047=CARTESIAN_POINT('Ctrl Pts',(-97.3220593832045,-139.962224365005,
-82.9469649889257));
#23048=CARTESIAN_POINT('Ctrl Pts',(-95.9760732771133,-140.316081550096,
-83.6111084029453));
#23049=CARTESIAN_POINT('Ctrl Pts',(-96.6060933643896,-139.88514399948,-83.3040436736954));
#23050=CARTESIAN_POINT('Ctrl Pts',(-97.3877326179702,-139.939793891199,
-83.0554758102092));
#23051=CARTESIAN_POINT('Ctrl Pts',(-96.1359171968624,-140.206614708383,
-84.0186285797908));
#23052=CARTESIAN_POINT('Ctrl Pts',(-96.7586808353661,-139.779598324237,
-83.5942322269066));
#23053=CARTESIAN_POINT('Ctrl Pts',(-97.5499289003671,-139.884271165605,
-83.2592091881112));
#23054=CARTESIAN_POINT('Ctrl Pts',(-96.2312574439685,-140.141222656174,
-84.2116073129497));
#23055=CARTESIAN_POINT('Ctrl Pts',(-96.8497861981093,-139.716486932324,
-83.7303149679426));
#23056=CARTESIAN_POINT('Ctrl Pts',(-97.6466721866358,-139.851103576304,
-83.3556865024526));
#23057=CARTESIAN_POINT('Ctrl Pts',(-96.4473504048935,-139.992591935039,
-84.5797041056106));
#23058=CARTESIAN_POINT('Ctrl Pts',(-97.0555509298913,-139.573566933705,
-83.9861341719472));
#23059=CARTESIAN_POINT('Ctrl Pts',(-97.8659453704935,-139.775715999607,
-83.5397134594334));
#23060=CARTESIAN_POINT('Ctrl Pts',(-96.5679243919286,-139.909470610044,
-84.753989376282));
#23061=CARTESIAN_POINT('Ctrl Pts',(-97.1703586838473,-139.493647616232,
-84.1053449302004));
#23062=CARTESIAN_POINT('Ctrl Pts',(-97.988293803748,-139.733555567923,-83.6268467456611));
#23063=CARTESIAN_POINT('Ctrl Pts',(-96.9500803569865,-139.645185630461,
-85.2398999355243));
#23064=CARTESIAN_POINT('Ctrl Pts',(-97.5346293970093,-139.239315047688,
-84.432869704325));
#23065=CARTESIAN_POINT('Ctrl Pts',(-98.3760735528373,-139.599505523372,
-83.869778159324));
#23066=CARTESIAN_POINT('Ctrl Pts',(-97.2354525040936,-139.446786719831,
-85.5216876072799));
#23067=CARTESIAN_POINT('Ctrl Pts',(-97.8055901602077,-139.049145300856,
-84.6129417193589));
#23068=CARTESIAN_POINT('Ctrl Pts',(-98.6656453772933,-139.498873185455,
-84.0106618938592));
#23069=CARTESIAN_POINT('Ctrl Pts',(-97.8473613034821,-139.018104706213,
-86.0240708677861));
#23070=CARTESIAN_POINT('Ctrl Pts',(-98.3809815624785,-138.642451119717,
-84.9145219274105));
#23071=CARTESIAN_POINT('Ctrl Pts',(-99.2865604725273,-139.281432946433,
-84.261842700229));
#23072=CARTESIAN_POINT('Ctrl Pts',(-98.166043362077,-138.793333891558,-86.2379611602896));
#23073=CARTESIAN_POINT('Ctrl Pts',(-98.6796642081939,-138.429941914644,
-85.0311843476496));
#23074=CARTESIAN_POINT('Ctrl Pts',(-99.6099329912234,-139.167421255508,
-84.3687873468957));
#23075=CARTESIAN_POINT('Ctrl Pts',(-98.8213488187872,-138.327519386904,
-86.6110898616107));
#23076=CARTESIAN_POINT('Ctrl Pts',(-99.2879449246068,-137.99409288667,-85.2121201908135));
#23077=CARTESIAN_POINT('Ctrl Pts',(-100.27488438625,-138.931140045818,-84.5553582822015));
#23078=CARTESIAN_POINT('Ctrl Pts',(-99.158096702725,-138.086393592506,-86.7699896797119));
#23079=CARTESIAN_POINT('Ctrl Pts',(-99.5988267512419,-137.769758011627,
-85.2749349361932));
#23080=CARTESIAN_POINT('Ctrl Pts',(-100.616589177682,-138.808829045632,
-84.6348154491461));
#23081=CARTESIAN_POINT('Ctrl Pts',(-99.8465457819727,-137.589416498872,
-87.0407064600204));
#23082=CARTESIAN_POINT('Ctrl Pts',(-100.226641408904,-137.313468734571,
-85.3520865086701));
#23083=CARTESIAN_POINT('Ctrl Pts',(-101.315173303503,-138.556733152654,
-84.7701949757435));
#23084=CARTESIAN_POINT('Ctrl Pts',(-100.196958385718,-137.33447257932,-87.1516264431987));
#23085=CARTESIAN_POINT('Ctrl Pts',(-100.543205603967,-137.081667395925,
-85.3644982653947));
#23086=CARTESIAN_POINT('Ctrl Pts',(-101.670744758199,-138.427408643402,
-84.825669005131));
#23087=CARTESIAN_POINT('Ctrl Pts',(-101.28821838667,-136.53403653485,-87.424812055919));
#23088=CARTESIAN_POINT('Ctrl Pts',(-101.533114418462,-136.351795325561,
-85.3295920701886));
#23089=CARTESIAN_POINT('Ctrl Pts',(-102.778066848943,-138.021368555811,
-84.9623127946849));
#23090=CARTESIAN_POINT('Ctrl Pts',(-102.034252820327,-135.97755865104,-87.5102062320114));
#23091=CARTESIAN_POINT('Ctrl Pts',(-102.179857181136,-135.866853574869,
-85.1905835679741));
#23092=CARTESIAN_POINT('Ctrl Pts',(-103.535087152147,-137.73907034878,-85.0050578474458));
#23093=CARTESIAN_POINT('Ctrl Pts',(-102.783621163517,-135.408741267554,
-87.4990307673126));
#23094=CARTESIAN_POINT('Ctrl Pts',(-102.759250409398,-135.427238236657,
-84.9584361067278));
#23095=CARTESIAN_POINT('Ctrl Pts',(-104.295502567802,-137.450494181459,
-84.9995248789654));
#23096=CARTESIAN_POINT('Origin',(-97.2111104761179,-142.5,-82.5));
#23097=CARTESIAN_POINT('Origin',(-168.964466094067,-137.5,82.5));
#23098=CARTESIAN_POINT('Origin',(-168.964466094067,-137.5,82.5));
#23099=CARTESIAN_POINT('Origin',(-168.964466094067,-137.5,82.5));
#23100=CARTESIAN_POINT('Origin',(-177.5,-127.5,73.9644660940671));
#23101=CARTESIAN_POINT('Origin',(-177.5,-127.5,73.9644660940671));
#23102=CARTESIAN_POINT('Origin',(-97.2111104761179,-142.5,115.));
#23103=CARTESIAN_POINT('Origin',(-97.2111104761179,-142.5,82.5));
#23104=CARTESIAN_POINT('Origin',(0.,-137.5,82.5));
#23105=CARTESIAN_POINT('Ctrl Pts',(-104.163333279998,-137.5,85.));
#23106=CARTESIAN_POINT('Ctrl Pts',(-103.738099080441,-137.661068405961,
85.));
#23107=CARTESIAN_POINT('Ctrl Pts',(-103.313784132472,-137.820236149174,
84.9848502161634));
#23108=CARTESIAN_POINT('Ctrl Pts',(-102.890445132596,-137.977529707376,
84.9541805579568));
#23109=CARTESIAN_POINT('Ctrl Pts',(-102.674532847161,-138.057752913,84.9385383515953));
#23110=CARTESIAN_POINT('Ctrl Pts',(-102.458874713662,-138.137488523029,
84.9188583125581));
#23111=CARTESIAN_POINT('Ctrl Pts',(-102.243480097268,-138.216739650426,
84.8950864427477));
#23112=CARTESIAN_POINT('Ctrl Pts',(-102.169808729557,-138.243845894054,
84.8869557559584));
#23113=CARTESIAN_POINT('Ctrl Pts',(-102.096197177396,-138.270885582569,
84.8783493800412));
#23114=CARTESIAN_POINT('Ctrl Pts',(-102.022632569934,-138.297863659494,
84.8692643545073));
#23115=CARTESIAN_POINT('Ctrl Pts',(-101.824799549342,-138.370414232822,
84.8448325236913));
#23116=CARTESIAN_POINT('Ctrl Pts',(-101.627311999894,-138.442516995573,
84.8168822159707));
#23117=CARTESIAN_POINT('Ctrl Pts',(-101.42999704102,-138.514238577898,84.7850438375703));
#23118=CARTESIAN_POINT('Ctrl Pts',(-101.276966125295,-138.569863450352,
84.7603510508216));
#23119=CARTESIAN_POINT('Ctrl Pts',(-101.124039180306,-138.625258921571,
84.7333188027895));
#23120=CARTESIAN_POINT('Ctrl Pts',(-100.971140292634,-138.680453268945,
84.7037536341508));
#23121=CARTESIAN_POINT('Ctrl Pts',(-100.819413206494,-138.735224612453,
84.6744150499591));
#23122=CARTESIAN_POINT('Ctrl Pts',(-100.667483749192,-138.789877248555,
84.6424995110724));
#23123=CARTESIAN_POINT('Ctrl Pts',(-100.516166836934,-138.844125833747,
84.6079054671296));
#23124=CARTESIAN_POINT('Ctrl Pts',(-100.456828089701,-138.865399351931,
84.5943394539282));
#23125=CARTESIAN_POINT('Ctrl Pts',(-100.397584005817,-138.886610562357,
84.5803613497262));
#23126=CARTESIAN_POINT('Ctrl Pts',(-100.338485741259,-138.907741516914,
84.565964289852));
#23127=CARTESIAN_POINT('Ctrl Pts',(-100.220918177777,-138.949778535426,
84.5373233938226));
#23128=CARTESIAN_POINT('Ctrl Pts',(-100.103632370179,-138.991604254091,
84.5069540658058));
#23129=CARTESIAN_POINT('Ctrl Pts',(-99.9869935660692,-139.033088789031,
84.4747498712919));
#23130=CARTESIAN_POINT('Ctrl Pts',(-99.9720326094956,-139.038409902621,
84.4706191228734));
#23131=CARTESIAN_POINT('Ctrl Pts',(-99.9570823608136,-139.043725379489,
84.4664581642972));
#23132=CARTESIAN_POINT('Ctrl Pts',(-99.9421436485644,-139.049034924161,
84.4622667514209));
#23133=CARTESIAN_POINT('Ctrl Pts',(-99.8232112700053,-139.0913060896,84.4288974291803));
#23134=CARTESIAN_POINT('Ctrl Pts',(-99.7047475328351,-139.133296386698,
84.3935836754955));
#23135=CARTESIAN_POINT('Ctrl Pts',(-99.5868591110941,-139.174972397689,
84.3559924242641));
#23136=CARTESIAN_POINT('Ctrl Pts',(-99.5255437217676,-139.196648664126,
84.336440697551));
#23137=CARTESIAN_POINT('Ctrl Pts',(-99.4643844621158,-139.218239730484,
84.3162722626081));
#23138=CARTESIAN_POINT('Ctrl Pts',(-99.4033998553792,-139.239739634851,
84.2954359997591));
#23139=CARTESIAN_POINT('Ctrl Pts',(-99.3132315996693,-139.271528129989,
84.2646287259707));
#23140=CARTESIAN_POINT('Ctrl Pts',(-99.223535776852,-139.303085592255,84.2323955368028));
#23141=CARTESIAN_POINT('Ctrl Pts',(-99.1342049110009,-139.334451631701,
84.1984942631106));
#23142=CARTESIAN_POINT('Ctrl Pts',(-99.0808040909447,-139.353201838725,
84.1782285263033));
#23143=CARTESIAN_POINT('Ctrl Pts',(-99.0275342339471,-139.371883428182,
84.1573660209767));
#23144=CARTESIAN_POINT('Ctrl Pts',(-98.9743778992268,-139.390502757733,
84.1358481968094));
#23145=CARTESIAN_POINT('Ctrl Pts',(-98.8981671957289,-139.417197453882,
84.1049979034971));
#23146=CARTESIAN_POINT('Ctrl Pts',(-98.8224769045325,-139.443662996202,
84.0729177573328));
#23147=CARTESIAN_POINT('Ctrl Pts',(-98.7474387368693,-139.46985661819,84.0394249607335));
#23148=CARTESIAN_POINT('Ctrl Pts',(-98.6761330066818,-139.4947473558,84.0075981132516));
#23149=CARTESIAN_POINT('Ctrl Pts',(-98.6054159170073,-139.519392616372,
83.9744956741588));
#23150=CARTESIAN_POINT('Ctrl Pts',(-98.5354408951835,-139.543741578814,
83.9399393538181));
#23151=CARTESIAN_POINT('Ctrl Pts',(-98.5230520237326,-139.548052490877,
83.9338212591129));
#23152=CARTESIAN_POINT('Ctrl Pts',(-98.5106865249416,-139.552354076384,
83.9276575341684));
#23153=CARTESIAN_POINT('Ctrl Pts',(-98.4983453996891,-139.556646001529,
83.921447113738));
#23154=CARTESIAN_POINT('Ctrl Pts',(-98.4332103940779,-139.579298276965,
83.8886692461367));
#23155=CARTESIAN_POINT('Ctrl Pts',(-98.3686986921717,-139.601700795348,
83.8545667766362));
#23156=CARTESIAN_POINT('Ctrl Pts',(-98.3049498142096,-139.623806785601,
83.8189431096019));
#23157=CARTESIAN_POINT('Ctrl Pts',(-98.2461451146523,-139.644198299252,
83.7860823110428));
#23158=CARTESIAN_POINT('Ctrl Pts',(-98.1879895705334,-139.664337465922,
83.7519270259336));
#23159=CARTESIAN_POINT('Ctrl Pts',(-98.1306351301536,-139.684172991867,
83.7163018099732));
#23160=CARTESIAN_POINT('Ctrl Pts',(-98.1258128865628,-139.685840722163,
83.7133065149586));
#23161=CARTESIAN_POINT('Ctrl Pts',(-98.1209963324925,-139.687506296946,
83.710300816007));
#23162=CARTESIAN_POINT('Ctrl Pts',(-98.1161855731307,-139.689169680641,
83.7072846016472));
#23163=CARTESIAN_POINT('Ctrl Pts',(-98.1011329199801,-139.694374334612,
83.697847000393));
#23164=CARTESIAN_POINT('Ctrl Pts',(-98.0861233722941,-139.699562258723,
83.6882946516978));
#23165=CARTESIAN_POINT('Ctrl Pts',(-98.0711656112444,-139.704730507617,
83.6786258523484));
#23166=CARTESIAN_POINT('Ctrl Pts',(-98.0285985107537,-139.719438415389,
83.6511101865903));
#23167=CARTESIAN_POINT('Ctrl Pts',(-97.9864063827793,-139.734002420143,
83.6226254451987));
#23168=CARTESIAN_POINT('Ctrl Pts',(-97.9447745948348,-139.748359981237,
83.5930927466016));
#23169=CARTESIAN_POINT('Ctrl Pts',(-97.9055854441768,-139.761875149636,
83.5652928025733));
#23170=CARTESIAN_POINT('Ctrl Pts',(-97.8668926229667,-139.775207447803,
83.5365641602674));
#23171=CARTESIAN_POINT('Ctrl Pts',(-97.828893412403,-139.788290019043,83.5068350472078));
#23172=CARTESIAN_POINT('Ctrl Pts',(-97.804144005828,-139.796810876973,83.4874720684692));
#23173=CARTESIAN_POINT('Ctrl Pts',(-97.7796896932354,-139.805225503118,
83.4676845636184));
#23174=CARTESIAN_POINT('Ctrl Pts',(-97.7555963200441,-139.813511537342,
83.4474515115311));
#23175=CARTESIAN_POINT('Ctrl Pts',(-97.728363634325,-139.822877223255,83.424582138104));
#23176=CARTESIAN_POINT('Ctrl Pts',(-97.7016349752933,-139.832064017308,
83.4011923028985));
#23177=CARTESIAN_POINT('Ctrl Pts',(-97.6754851218662,-139.841046916235,
83.3772268830841));
#23178=CARTESIAN_POINT('Ctrl Pts',(-97.6463215006398,-139.851065093299,
83.3504994512098));
#23179=CARTESIAN_POINT('Ctrl Pts',(-97.6179056267942,-139.860816746996,
83.3230936650656));
#23180=CARTESIAN_POINT('Ctrl Pts',(-97.5902935806194,-139.87028550355,83.2948558990642));
#23181=CARTESIAN_POINT('Ctrl Pts',(-97.5639466259767,-139.879320433372,
83.2679118929831));
#23182=CARTESIAN_POINT('Ctrl Pts',(-97.5383314014496,-139.88809782761,83.2402104364255));
#23183=CARTESIAN_POINT('Ctrl Pts',(-97.5135388526037,-139.896588714057,
83.2116040346635));
#23184=CARTESIAN_POINT('Ctrl Pts',(-97.4980774724969,-139.901883886554,
83.1937642210211));
#23185=CARTESIAN_POINT('Ctrl Pts',(-97.4829368794924,-139.907067340337,
83.17557218315));
#23186=CARTESIAN_POINT('Ctrl Pts',(-97.4681484941753,-139.91212881033,83.1569890466364));
#23187=CARTESIAN_POINT('Ctrl Pts',(-97.4476130510072,-139.919157267269,
83.1311841372042));
#23188=CARTESIAN_POINT('Ctrl Pts',(-97.4277452420287,-139.925954449789,
83.1045520895884));
#23189=CARTESIAN_POINT('Ctrl Pts',(-97.4087167048375,-139.932462814289,
83.0770775195449));
#23190=CARTESIAN_POINT('Ctrl Pts',(-97.3896881676464,-139.938971178789,
83.0496029495014));
#23191=CARTESIAN_POINT('Ctrl Pts',(-97.3714983087636,-139.945190921619,
83.0212855162084));
#23192=CARTESIAN_POINT('Ctrl Pts',(-97.3543677310461,-139.951047779757,
82.9921212813803));
#23193=CARTESIAN_POINT('Ctrl Pts',(-97.3386981110691,-139.956405143811,
82.9654442781753));
#23194=CARTESIAN_POINT('Ctrl Pts',(-97.3240367075897,-139.961419891151,
82.9382531572));
#23195=CARTESIAN_POINT('Ctrl Pts',(-97.3105164866214,-139.966044132201,
82.910533567852));
#23196=CARTESIAN_POINT('Ctrl Pts',(-97.2987364265489,-139.970073196333,
82.8863817120154));
#23197=CARTESIAN_POINT('Ctrl Pts',(-97.2878230738592,-139.973805693467,
82.8618285577111));
#23198=CARTESIAN_POINT('Ctrl Pts',(-97.277894901901,-139.977199920877,82.8368687469214));
#23199=CARTESIAN_POINT('Ctrl Pts',(-97.2675449135807,-139.980738358185,
82.8108484733772));
#23200=CARTESIAN_POINT('Ctrl Pts',(-97.2582088704294,-139.983928680802,
82.7843403311583));
#23201=CARTESIAN_POINT('Ctrl Pts',(-97.2499984542927,-139.986731261435,
82.757268617013));
#23202=CARTESIAN_POINT('Ctrl Pts',(-97.2412356636815,-139.989722392072,
82.7283755915447));
#23203=CARTESIAN_POINT('Ctrl Pts',(-97.2338238173965,-139.992251733102,
82.6990112555058));
#23204=CARTESIAN_POINT('Ctrl Pts',(-97.2279126563665,-139.99426861304,82.6692964230559));
#23205=CARTESIAN_POINT('Ctrl Pts',(-97.2221710252593,-139.996227649603,
82.6404338010639));
#23206=CARTESIAN_POINT('Ctrl Pts',(-97.2178453353219,-139.997703166035,
82.6112405024812));
#23207=CARTESIAN_POINT('Ctrl Pts',(-97.2150271728466,-139.998664330779,
82.5818324954324));
#23208=CARTESIAN_POINT('Ctrl Pts',(-97.21242764044,-139.999550929378,82.5547059305124));
#23209=CARTESIAN_POINT('Ctrl Pts',(-97.2111104751974,-140.,82.5273967255209));
#23210=CARTESIAN_POINT('Ctrl Pts',(-97.2111104761178,-140.,82.5));
#23211=CARTESIAN_POINT('Origin',(-168.964466094067,0.,82.5));
#23212=CARTESIAN_POINT('Origin',(-168.964466094067,-127.5,82.5));
#23213=CARTESIAN_POINT('Origin',(-140.840826156048,-127.5,110.623639938019));
#23214=CARTESIAN_POINT('Origin',(-168.964466094067,-127.5,82.5));
#23215=CARTESIAN_POINT('Origin',(0.,-122.5,32.5));
#23216=CARTESIAN_POINT('Origin',(-147.5,-122.5,32.5));
#23217=CARTESIAN_POINT('Origin',(-121.449578014911,-122.5,115.));
#23218=CARTESIAN_POINT('Ctrl Pts',(-102.653719754201,-135.507246376812,
87.5));
#23219=CARTESIAN_POINT('Ctrl Pts',(-102.653719754201,-135.507246376812,
85.));
#23220=CARTESIAN_POINT('Ctrl Pts',(-104.163333279998,-137.5,85.));
#23221=CARTESIAN_POINT('Ctrl Pts',(-101.942824967883,-136.045785799024,
87.4999999986499));
#23222=CARTESIAN_POINT('Ctrl Pts',(-102.098115024429,-135.928145581712,
85.2088536164867));
#23223=CARTESIAN_POINT('Ctrl Pts',(-103.441984205064,-137.773229542126,
85.));
#23224=CARTESIAN_POINT('Ctrl Pts',(-101.239352594638,-136.569897864386,
87.412786288228));
#23225=CARTESIAN_POINT('Ctrl Pts',(-101.486609565828,-136.386099347641,
85.331905314613));
#23226=CARTESIAN_POINT('Ctrl Pts',(-102.728166603362,-138.039139357556,
84.9563931437868));
#23227=CARTESIAN_POINT('Ctrl Pts',(-100.196407749732,-137.334867215748,
87.1513844296707));
#23228=CARTESIAN_POINT('Ctrl Pts',(-100.54257036391,-137.08212804413,85.3647787687136));
#23229=CARTESIAN_POINT('Ctrl Pts',(-101.669884334297,-138.427248808045,
84.825692214999));
#23230=CARTESIAN_POINT('Ctrl Pts',(-99.8508244887539,-137.58630689324,87.0421034532917));
#23231=CARTESIAN_POINT('Ctrl Pts',(-100.230398916982,-137.310719986095,
85.3526237075885));
#23232=CARTESIAN_POINT('Ctrl Pts',(-101.319218966522,-138.554817467693,
84.7710517262891));
#23233=CARTESIAN_POINT('Ctrl Pts',(-99.1647702284533,-138.081596677989,
86.7728948774191));
#23234=CARTESIAN_POINT('Ctrl Pts',(-99.6048287382421,-137.765412086316,
85.2762415031115));
#23235=CARTESIAN_POINT('Ctrl Pts',(-100.623075672997,-138.806104197121,
84.6364474390664));
#23236=CARTESIAN_POINT('Ctrl Pts',(-98.8231223087188,-138.326258685221,
86.6120988871654));
#23237=CARTESIAN_POINT('Ctrl Pts',(-99.2895441365193,-137.992946799803,
85.2128933853019));
#23238=CARTESIAN_POINT('Ctrl Pts',(-100.276403519106,-138.930234185559,
84.5560494432021));
#23239=CARTESIAN_POINT('Ctrl Pts',(-98.1642932033775,-138.794578008566,
86.236965419431));
#23240=CARTESIAN_POINT('Ctrl Pts',(-98.6779850295722,-138.431144249613,
85.0309421888964));
#23241=CARTESIAN_POINT('Ctrl Pts',(-99.6078857505209,-139.167837372319,
84.3684827100962));
#23242=CARTESIAN_POINT('Ctrl Pts',(-97.8450871550092,-139.019702589725,
86.0223563343333));
#23243=CARTESIAN_POINT('Ctrl Pts',(-98.3787305056279,-138.644046161722,
84.9137267915435));
#23244=CARTESIAN_POINT('Ctrl Pts',(-99.283985495488,-139.28205498953,84.2611781664592));
#23245=CARTESIAN_POINT('Ctrl Pts',(-97.2348460956408,-139.447206832062,
85.5210364529044));
#23246=CARTESIAN_POINT('Ctrl Pts',(-97.8048933229574,-139.049632684085,
84.6126732163398));
#23247=CARTESIAN_POINT('Ctrl Pts',(-98.6647703029657,-139.498950525936,
84.0105182271597));
#23248=CARTESIAN_POINT('Ctrl Pts',(-96.9485250987458,-139.646264128654,
85.2381599055602));
#23249=CARTESIAN_POINT('Ctrl Pts',(-97.5330426499524,-139.240425205481,
84.4318673801205));
#23250=CARTESIAN_POINT('Ctrl Pts',(-98.3742387030706,-139.599942828535,
83.869079952008));
#23251=CARTESIAN_POINT('Ctrl Pts',(-96.5670588723941,-139.910067692477,
84.7527693623909));
#23252=CARTESIAN_POINT('Ctrl Pts',(-97.1694267365962,-139.49429609941,84.1046276840804));
#23253=CARTESIAN_POINT('Ctrl Pts',(-97.9871626793753,-139.7337843447,83.6263846815815));
#23254=CARTESIAN_POINT('Ctrl Pts',(-96.446921948779,-139.992887137954,84.5790592166605));
#23255=CARTESIAN_POINT('Ctrl Pts',(-97.0550355767484,-139.573924747954,
83.985796851679));
#23256=CARTESIAN_POINT('Ctrl Pts',(-97.8652590362145,-139.775803032622,
83.5395296080959));
#23257=CARTESIAN_POINT('Ctrl Pts',(-96.230792082191,-140.141542227306,84.2107293038302));
#23258=CARTESIAN_POINT('Ctrl Pts',(-96.8492338219199,-139.716869275045,
83.7297846724926));
#23259=CARTESIAN_POINT('Ctrl Pts',(-97.6459507893286,-139.851223630635,
83.3553646521495));
#23260=CARTESIAN_POINT('Ctrl Pts',(-96.1354852319174,-140.20691083986,84.0176816842604));
#23261=CARTESIAN_POINT('Ctrl Pts',(-96.7581590378938,-139.779958879001,
83.5936364082725));
#23262=CARTESIAN_POINT('Ctrl Pts',(-97.5492423676424,-139.884388586841,
83.2588408418563));
#23263=CARTESIAN_POINT('Ctrl Pts',(-95.9757708369295,-140.316288364145,
83.6101822300658));
#23264=CARTESIAN_POINT('Ctrl Pts',(-96.6056940387067,-139.885419084152,
83.3034331025056));
#23265=CARTESIAN_POINT('Ctrl Pts',(-97.3871792316287,-139.939881597544,
83.0550911153068));
#23266=CARTESIAN_POINT('Ctrl Pts',(-95.9112233305706,-140.360393155342,
83.3934903679299));
#23267=CARTESIAN_POINT('Ctrl Pts',(-96.5438567051695,-139.928100230385,
83.1474982708776));
#23268=CARTESIAN_POINT('Ctrl Pts',(-97.3216824971681,-139.962258291636,
82.9467451839126));
#23269=CARTESIAN_POINT('Ctrl Pts',(-95.8249655550993,-140.419296052404,
82.9539654903595));
#23270=CARTESIAN_POINT('Ctrl Pts',(-96.4613838167463,-139.984990149168,
82.8298756349127));
#23271=CARTESIAN_POINT('Ctrl Pts',(-97.2341562250557,-139.99214285053,82.7269827452321));
#23272=CARTESIAN_POINT('Ctrl Pts',(-95.802253798755,-140.434782611285,82.7294636530625));
#23273=CARTESIAN_POINT('Ctrl Pts',(-96.4395937226627,-140.0000000025,82.6666388430675));
#23274=CARTESIAN_POINT('Ctrl Pts',(-97.2111104722631,-140.,82.6147318264911));
#23275=CARTESIAN_POINT('Ctrl Pts',(-95.802253802551,-140.434782608696,82.5));
#23276=CARTESIAN_POINT('Ctrl Pts',(-96.4395937263074,-140.,82.5));
#23277=CARTESIAN_POINT('Ctrl Pts',(-97.2111104761179,-140.,82.5));
#23278=CARTESIAN_POINT('Origin',(-104.163333279998,-137.5,87.5));
#23279=CARTESIAN_POINT('Origin',(-168.964466094067,-127.5,82.5));
#23280=CARTESIAN_POINT('Origin',(-168.964466094067,-127.5,82.5));
#23281=CARTESIAN_POINT('Origin',(-147.5,-122.5,37.5));
#23282=CARTESIAN_POINT('Origin',(-152.5,-122.5,37.5));
#23283=CARTESIAN_POINT('Origin',(-147.5,-122.5,37.5));
#23284=CARTESIAN_POINT('Origin',(0.,0.,87.5));
#23285=CARTESIAN_POINT('Origin',(-116.189500386222,-127.5,87.5));
#23286=CARTESIAN_POINT('Origin',(0.,-127.5,82.5));
#23287=CARTESIAN_POINT('Ctrl Pts',(-121.449578014911,-125.,82.5));
#23288=CARTESIAN_POINT('Ctrl Pts',(-121.449578013665,-125.,82.5578430303778));
#23289=CARTESIAN_POINT('Ctrl Pts',(-121.445542821646,-125.002000739816,
82.6149744276206));
#23290=CARTESIAN_POINT('Ctrl Pts',(-121.437730668306,-125.005872173714,
82.6713216462766));
#23291=CARTESIAN_POINT('Ctrl Pts',(-121.431548654752,-125.008935766527,
82.7159110513069));
#23292=CARTESIAN_POINT('Ctrl Pts',(-121.423002583494,-125.013170255242,
82.760009542539));
#23293=CARTESIAN_POINT('Ctrl Pts',(-121.412240896123,-125.018501093781,
82.8035838902947));
#23294=CARTESIAN_POINT('Ctrl Pts',(-121.402625881463,-125.023263924083,
82.8425153308796));
#23295=CARTESIAN_POINT('Ctrl Pts',(-121.391240873519,-125.02890257476,82.8810286286794));
#23296=CARTESIAN_POINT('Ctrl Pts',(-121.378166904503,-125.035375090082,
82.9190974411551));
#23297=CARTESIAN_POINT('Ctrl Pts',(-121.359482649641,-125.044625083389,
82.9735022966162));
#23298=CARTESIAN_POINT('Ctrl Pts',(-121.337601423089,-125.055455126064,
83.0262941391223));
#23299=CARTESIAN_POINT('Ctrl Pts',(-121.312984159938,-125.067631742438,
83.0775690600153));
#23300=CARTESIAN_POINT('Ctrl Pts',(-121.309754155107,-125.069229423281,
83.0842967876761));
#23301=CARTESIAN_POINT('Ctrl Pts',(-121.306476982697,-125.070850319854,
83.0909983906631));
#23302=CARTESIAN_POINT('Ctrl Pts',(-121.303153626062,-125.072493934659,
83.0976740773907));
#23303=CARTESIAN_POINT('Ctrl Pts',(-121.28333698938,-125.082294543202,83.1374801147826));
#23304=CARTESIAN_POINT('Ctrl Pts',(-121.26193952168,-125.092872330006,83.17618707187));
#23305=CARTESIAN_POINT('Ctrl Pts',(-121.239293756531,-125.104060083144,
83.2137354525194));
#23306=CARTESIAN_POINT('Ctrl Pts',(-121.223112895711,-125.112053960817,
83.2405645358964));
#23307=CARTESIAN_POINT('Ctrl Pts',(-121.206293748505,-125.120359745354,
83.2668025986261));
#23308=CARTESIAN_POINT('Ctrl Pts',(-121.188944294236,-125.128923152136,
83.2924342403752));
#23309=CARTESIAN_POINT('Ctrl Pts',(-121.169248714547,-125.138644568041,
83.3215319880497));
#23310=CARTESIAN_POINT('Ctrl Pts',(-121.148816846868,-125.14872481678,83.3499289055538));
#23311=CARTESIAN_POINT('Ctrl Pts',(-121.127768696513,-125.159103720469,
83.3776130175156));
#23312=CARTESIAN_POINT('Ctrl Pts',(-121.095198113589,-125.175164368916,
83.4204523002623));
#23313=CARTESIAN_POINT('Ctrl Pts',(-121.06107241282,-125.191979398505,83.4617485539175));
#23314=CARTESIAN_POINT('Ctrl Pts',(-121.025604781292,-125.209440222843,
83.501677334517));
#23315=CARTESIAN_POINT('Ctrl Pts',(-120.994690465973,-125.224659435575,
83.536480078894));
#23316=CARTESIAN_POINT('Ctrl Pts',(-120.962755773204,-125.240369726302,
83.5702435568607));
#23317=CARTESIAN_POINT('Ctrl Pts',(-120.929914941896,-125.256512858459,
83.6030728931431));
#23318=CARTESIAN_POINT('Ctrl Pts',(-120.919024936224,-125.261865914206,
83.6139590870702));
#23319=CARTESIAN_POINT('Ctrl Pts',(-120.908034223584,-125.267267022157,
83.6247432148631));
#23320=CARTESIAN_POINT('Ctrl Pts',(-120.896946618515,-125.272714234811,
83.6354286063845));
#23321=CARTESIAN_POINT('Ctrl Pts',(-120.861818540488,-125.289972254912,
83.6692823795648));
#23322=CARTESIAN_POINT('Ctrl Pts',(-120.825696080648,-125.307703371905,
83.7021357945799));
#23323=CARTESIAN_POINT('Ctrl Pts',(-120.788855644393,-125.325770196084,
83.7339645608881));
#23324=CARTESIAN_POINT('Ctrl Pts',(-120.750104876469,-125.344773861135,
83.7674437826873));
#23325=CARTESIAN_POINT('Ctrl Pts',(-120.710559563375,-125.364149043196,
83.7997894992622));
#23326=CARTESIAN_POINT('Ctrl Pts',(-120.670490053905,-125.383761285265,
83.8309820047453));
#23327=CARTESIAN_POINT('Ctrl Pts',(-120.655933159393,-125.390886237448,
83.8423139630822));
#23328=CARTESIAN_POINT('Ctrl Pts',(-120.64130662474,-125.398042702867,83.8534937861157));
#23329=CARTESIAN_POINT('Ctrl Pts',(-120.62662193437,-125.405224965794,83.8645207217807));
#23330=CARTESIAN_POINT('Ctrl Pts',(-120.623763587428,-125.406622979559,
83.8666670937534));
#23331=CARTESIAN_POINT('Ctrl Pts',(-120.62090288229,-125.40802204969,83.8688077929118));
#23332=CARTESIAN_POINT('Ctrl Pts',(-120.618039908549,-125.409422131597,
83.8709428055742));
#23333=CARTESIAN_POINT('Ctrl Pts',(-120.561761358576,-125.436944067424,
83.9129115512495));
#23334=CARTESIAN_POINT('Ctrl Pts',(-120.504422162934,-125.464947521895,
83.9528770557974));
#23335=CARTESIAN_POINT('Ctrl Pts',(-120.446193115434,-125.493345150898,
83.9910922510509));
#23336=CARTESIAN_POINT('Ctrl Pts',(-120.399258153872,-125.516234785589,
84.0218952402349));
#23337=CARTESIAN_POINT('Ctrl Pts',(-120.351744177112,-125.539380959607,
84.0515603444803));
#23338=CARTESIAN_POINT('Ctrl Pts',(-120.303722804547,-125.562746846771,
84.0802057525297));
#23339=CARTESIAN_POINT('Ctrl Pts',(-120.237604852662,-125.594918034739,
84.1196460186027));
#23340=CARTESIAN_POINT('Ctrl Pts',(-120.170523556422,-125.627506495568,
84.1571520519609));
#23341=CARTESIAN_POINT('Ctrl Pts',(-120.102573990086,-125.660461610429,
84.1929593090857));
#23342=CARTESIAN_POINT('Ctrl Pts',(-120.054961757025,-125.683553245799,
84.2180494393613));
#23343=CARTESIAN_POINT('Ctrl Pts',(-120.006922336468,-125.706825340362,
84.24230479924));
#23344=CARTESIAN_POINT('Ctrl Pts',(-119.958477373249,-125.73026591296,84.2657976274668));
#23345=CARTESIAN_POINT('Ctrl Pts',(-119.957432170273,-125.730771644714,
84.2663044866393));
#23346=CARTESIAN_POINT('Ctrl Pts',(-119.956386759699,-125.731277463805,
84.2668109935507));
#23347=CARTESIAN_POINT('Ctrl Pts',(-119.955341143413,-125.731783369317,
84.2673171481934));
#23348=CARTESIAN_POINT('Ctrl Pts',(-119.89298150186,-125.761955131908,84.2975037687741));
#23349=CARTESIAN_POINT('Ctrl Pts',(-119.829839678401,-125.792457959603,
84.3264634103549));
#23350=CARTESIAN_POINT('Ctrl Pts',(-119.766290102992,-125.823110100769,
84.3541852883538));
#23351=CARTESIAN_POINT('Ctrl Pts',(-119.706671564982,-125.85186616769,84.3801923517616));
#23352=CARTESIAN_POINT('Ctrl Pts',(-119.646693089753,-125.880754168446,
84.4051101569439));
#23353=CARTESIAN_POINT('Ctrl Pts',(-119.586626434295,-125.909641987124,
84.4289275235297));
#23354=CARTESIAN_POINT('Ctrl Pts',(-119.501128626528,-125.950760393823,
84.4628287390102));
#23355=CARTESIAN_POINT('Ctrl Pts',(-119.415197450965,-125.99200199476,84.4946555586857));
#23356=CARTESIAN_POINT('Ctrl Pts',(-119.328730569191,-126.033415379519,
84.524664540591));
#23357=CARTESIAN_POINT('Ctrl Pts',(-119.297298692445,-126.048469702963,
84.5355732099124));
#23358=CARTESIAN_POINT('Ctrl Pts',(-119.265795758865,-126.063546844264,
84.5462412487785));
#23359=CARTESIAN_POINT('Ctrl Pts',(-119.2342159707,-126.078649522118,84.5566796096831));
#23360=CARTESIAN_POINT('Ctrl Pts',(-119.130353069599,-126.12832078426,84.5910103797512));
#23361=CARTESIAN_POINT('Ctrl Pts',(-119.025943929888,-126.178130418089,
84.6227652061914));
#23362=CARTESIAN_POINT('Ctrl Pts',(-118.920995425666,-126.22807113596,84.6522643594009));
#23363=CARTESIAN_POINT('Ctrl Pts',(-118.879152593277,-126.247982435342,
84.6640256334899));
#23364=CARTESIAN_POINT('Ctrl Pts',(-118.8372237143,-126.267914711427,84.6754278512293));
#23365=CARTESIAN_POINT('Ctrl Pts',(-118.795208048995,-126.287868028778,
84.686489443114));
#23366=CARTESIAN_POINT('Ctrl Pts',(-118.687953257466,-126.338803528124,
84.7147267380122));
#23367=CARTESIAN_POINT('Ctrl Pts',(-118.579924099525,-126.389974247274,
84.740767917434));
#23368=CARTESIAN_POINT('Ctrl Pts',(-118.471295931314,-126.441294374187,
84.7647575879331));
#23369=CARTESIAN_POINT('Ctrl Pts',(-118.355734714551,-126.495889940035,
84.7902783672878));
#23370=CARTESIAN_POINT('Ctrl Pts',(-118.239495199037,-126.550654804871,
84.8134776148503));
#23371=CARTESIAN_POINT('Ctrl Pts',(-118.122742883405,-126.605505676004,
84.8344961206034));
#23372=CARTESIAN_POINT('Ctrl Pts',(-118.065228912442,-126.632526051511,
84.8448501570355));
#23373=CARTESIAN_POINT('Ctrl Pts',(-118.007589863346,-126.659567573612,
84.8546744803528));
#23374=CARTESIAN_POINT('Ctrl Pts',(-117.949842319794,-126.686621640134,
84.8639830042663));
#23375=CARTESIAN_POINT('Ctrl Pts',(-117.876606796367,-126.720931648849,
84.8757880885903));
#23376=CARTESIAN_POINT('Ctrl Pts',(-117.803387560177,-126.755173054075,
84.8867590613587));
#23377=CARTESIAN_POINT('Ctrl Pts',(-117.730135337144,-126.789368961517,
84.8969279885251));
#23378=CARTESIAN_POINT('Ctrl Pts',(-117.43068222065,-126.929160910906,84.9384982891291));
#23379=CARTESIAN_POINT('Ctrl Pts',(-117.129946637153,-127.068588179685,
84.9667803785313));
#23380=CARTESIAN_POINT('Ctrl Pts',(-116.828007609149,-127.207574667086,
84.9830546228536));
#23381=CARTESIAN_POINT('Ctrl Pts',(-116.615757670973,-127.305276092282,
84.9944947052243));
#23382=CARTESIAN_POINT('Ctrl Pts',(-116.402913049513,-127.402759565778,
85.));
#23383=CARTESIAN_POINT('Ctrl Pts',(-116.189500386222,-127.5,85.));
#23384=CARTESIAN_POINT('Origin',(-152.5,-122.5,85.));
#23385=CARTESIAN_POINT('Origin',(-152.5,-122.5,44.5));
#23386=CARTESIAN_POINT('Origin',(-147.5,-79.9999999999999,37.5));
#23387=CARTESIAN_POINT('Ctrl Pts',(-147.5,-89.4427190999916,35.));
#23388=CARTESIAN_POINT('Ctrl Pts',(-147.692029124165,-88.8093685912677,
35.));
#23389=CARTESIAN_POINT('Ctrl Pts',(-147.881019325443,-88.1768396525257,
35.0215706395343));
#23390=CARTESIAN_POINT('Ctrl Pts',(-148.067032921848,-87.5451886198136,
35.0650289614011));
#23391=CARTESIAN_POINT('Ctrl Pts',(-148.113199638031,-87.3884191442644,
35.0758148827002));
#23392=CARTESIAN_POINT('Ctrl Pts',(-148.159182993743,-87.2317038217301,
35.0879492852221));
#23393=CARTESIAN_POINT('Ctrl Pts',(-148.204983936061,-87.075043664733,35.1014374973017));
#23394=CARTESIAN_POINT('Ctrl Pts',(-148.227650188964,-86.9975147197269,
35.1081126269109));
#23395=CARTESIAN_POINT('Ctrl Pts',(-148.250265804087,-86.9200215223737,
35.1151175424361));
#23396=CARTESIAN_POINT('Ctrl Pts',(-148.272833473781,-86.8425552539348,
35.122453276526));
#23397=CARTESIAN_POINT('Ctrl Pts',(-148.349179005414,-86.5804899398114,
35.1472697740457));
#23398=CARTESIAN_POINT('Ctrl Pts',(-148.424974341849,-86.3187382386178,
35.1759312643052));
#23399=CARTESIAN_POINT('Ctrl Pts',(-148.500300623518,-86.0570314559301,
35.2088246089155));
#23400=CARTESIAN_POINT('Ctrl Pts',(-148.548487711945,-85.8896146181409,
35.2298668596451));
#23401=CARTESIAN_POINT('Ctrl Pts',(-148.596482723485,-85.7222162995132,
35.2526418166148));
#23402=CARTESIAN_POINT('Ctrl Pts',(-148.644305530043,-85.5547679896948,
35.2772618566301));
#23403=CARTESIAN_POINT('Ctrl Pts',(-148.705029122316,-85.3421484547101,
35.3085234529103));
#23404=CARTESIAN_POINT('Ctrl Pts',(-148.765481316906,-85.1294146681304,
35.3427818320249));
#23405=CARTESIAN_POINT('Ctrl Pts',(-148.825445173605,-84.9173615305793,
35.3802763717601));
#23406=CARTESIAN_POINT('Ctrl Pts',(-148.844370664369,-84.8504343861759,
35.3921102097507));
#23407=CARTESIAN_POINT('Ctrl Pts',(-148.863247416388,-84.7835753431863,
35.4042666138849));
#23408=CARTESIAN_POINT('Ctrl Pts',(-148.882068323811,-84.7168103169457,
35.4167536897855));
#23409=CARTESIAN_POINT('Ctrl Pts',(-148.922791444531,-84.5723496827009,
35.4437721904293));
#23410=CARTESIAN_POINT('Ctrl Pts',(-148.963298334261,-84.4281714850036,
35.4723673050235));
#23411=CARTESIAN_POINT('Ctrl Pts',(-149.003534667861,-84.2844711674245,
35.5026558877997));
#23412=CARTESIAN_POINT('Ctrl Pts',(-149.04618468001,-84.132150621731,35.5347614080551));
#23413=CARTESIAN_POINT('Ctrl Pts',(-149.088661184858,-83.9798999176192,
35.5688472728226));
#23414=CARTESIAN_POINT('Ctrl Pts',(-149.130874866098,-83.8280577825359,
35.6051699481661));
#23415=CARTESIAN_POINT('Ctrl Pts',(-149.15342877087,-83.7469316415681,35.6245764092162));
#23416=CARTESIAN_POINT('Ctrl Pts',(-149.175907457633,-83.6659227742899,
35.6446218400823));
#23417=CARTESIAN_POINT('Ctrl Pts',(-149.198295785931,-83.5850879913789,
35.6653487918288));
#23418=CARTESIAN_POINT('Ctrl Pts',(-149.22791298944,-83.4781527979922,35.692768183748));
#23419=CARTESIAN_POINT('Ctrl Pts',(-149.257371929283,-83.3715229740751,
35.7213784233686));
#23420=CARTESIAN_POINT('Ctrl Pts',(-149.286670239395,-83.2652102229956,
35.7513256082022));
#23421=CARTESIAN_POINT('Ctrl Pts',(-149.305367124994,-83.1973661276528,
35.7704365769474));
#23422=CARTESIAN_POINT('Ctrl Pts',(-149.32399829751,-83.1296521692792,35.7900922410059));
#23423=CARTESIAN_POINT('Ctrl Pts',(-149.342561050911,-83.0620783213206,
35.8103347154936));
#23424=CARTESIAN_POINT('Ctrl Pts',(-149.371267458519,-82.95757860723,35.8416387311796));
#23425=CARTESIAN_POINT('Ctrl Pts',(-149.399774767598,-82.8535435891935,
35.8742597573608));
#23426=CARTESIAN_POINT('Ctrl Pts',(-149.428061694081,-82.7500633861383,
35.9084779858675));
#23427=CARTESIAN_POINT('Ctrl Pts',(-149.454923581065,-82.6517963113765,
35.9409723675908));
#23428=CARTESIAN_POINT('Ctrl Pts',(-149.48158676368,-82.5540293874095,35.9749069410037));
#23429=CARTESIAN_POINT('Ctrl Pts',(-149.508023085914,-82.4568752753999,
36.0105521857142));
#23430=CARTESIAN_POINT('Ctrl Pts',(-149.512553176896,-82.4402270834618,
36.0166603046949));
#23431=CARTESIAN_POINT('Ctrl Pts',(-149.517076580988,-82.4235969779229,
36.0228187343148));
#23432=CARTESIAN_POINT('Ctrl Pts',(-149.521593124104,-82.406985643267,36.0290289363984));
#23433=CARTESIAN_POINT('Ctrl Pts',(-149.546047412515,-82.3170455368254,
36.0626533409386));
#23434=CARTESIAN_POINT('Ctrl Pts',(-149.570311794236,-82.2276143985463,
36.0978073544095));
#23435=CARTESIAN_POINT('Ctrl Pts',(-149.594353719118,-82.1388178247615,
36.1347461416596));
#23436=CARTESIAN_POINT('Ctrl Pts',(-149.612438155897,-82.0720246693601,
36.1625316524285));
#23437=CARTESIAN_POINT('Ctrl Pts',(-149.63039654831,-82.0055912015912,36.1913275605255));
#23438=CARTESIAN_POINT('Ctrl Pts',(-149.648211128679,-81.9395854582945,
36.2212549329038));
#23439=CARTESIAN_POINT('Ctrl Pts',(-149.655934224025,-81.9109702095313,
36.2342292463902));
#23440=CARTESIAN_POINT('Ctrl Pts',(-149.663637104736,-81.8824099165123,
36.2474379019948));
#23441=CARTESIAN_POINT('Ctrl Pts',(-149.67131055004,-81.8539394834478,36.2608852437835));
#23442=CARTESIAN_POINT('Ctrl Pts',(-149.685698655415,-81.8005559543076,
36.2860997026084));
#23443=CARTESIAN_POINT('Ctrl Pts',(-149.69999936079,-81.7474243597968,36.3121788856582));
#23444=CARTESIAN_POINT('Ctrl Pts',(-149.714175605302,-81.6946906272139,
36.3392201558208));
#23445=CARTESIAN_POINT('Ctrl Pts',(-149.727286670739,-81.6459192182506,
36.3642295906055));
#23446=CARTESIAN_POINT('Ctrl Pts',(-149.740291333114,-81.5974878781538,
36.3900621046248));
#23447=CARTESIAN_POINT('Ctrl Pts',(-149.75314895044,-81.5495528039286,36.4168048599562));
#23448=CARTESIAN_POINT('Ctrl Pts',(-149.76292982072,-81.5130882918069,36.4371482419517));
#23449=CARTESIAN_POINT('Ctrl Pts',(-149.772625404106,-81.4769116545281,
36.458018554439));
#23450=CARTESIAN_POINT('Ctrl Pts',(-149.782212501331,-81.4411109947051,
36.4794579384388));
#23451=CARTESIAN_POINT('Ctrl Pts',(-149.792712453297,-81.4019015030656,
36.5029387164987));
#23452=CARTESIAN_POINT('Ctrl Pts',(-149.80309231573,-81.3631061432697,36.5271022623878));
#23453=CARTESIAN_POINT('Ctrl Pts',(-149.813325028167,-81.3248298095044,
36.5520580116842));
#23454=CARTESIAN_POINT('Ctrl Pts',(-149.822817814989,-81.2893212306205,
36.5752092151911));
#23455=CARTESIAN_POINT('Ctrl Pts',(-149.832167251568,-81.2543175533046,
36.5989995466176));
#23456=CARTESIAN_POINT('Ctrl Pts',(-149.841373631764,-81.2198208404941,
36.623594471715));
#23457=CARTESIAN_POINT('Ctrl Pts',(-149.850444720927,-81.1858310691555,
36.6478279656349));
#23458=CARTESIAN_POINT('Ctrl Pts',(-149.859377062136,-81.1523329411744,
36.6728423499023));
#23459=CARTESIAN_POINT('Ctrl Pts',(-149.868158592942,-81.1193744240715,
36.6988172833931));
#23460=CARTESIAN_POINT('Ctrl Pts',(-149.876313696672,-81.0887669899376,
36.7229393051294));
#23461=CARTESIAN_POINT('Ctrl Pts',(-149.884338741479,-81.0586248955665,
36.7478897210636));
#23462=CARTESIAN_POINT('Ctrl Pts',(-149.8922125854,-81.0290296766823,36.773832259155));
#23463=CARTESIAN_POINT('Ctrl Pts',(-149.892817407753,-81.0267563461321,
36.7758250122624));
#23464=CARTESIAN_POINT('Ctrl Pts',(-149.893421331922,-81.0244862651329,
36.7778236297172));
#23465=CARTESIAN_POINT('Ctrl Pts',(-149.894024345238,-81.0222194822742,
36.7798281910486));
#23466=CARTESIAN_POINT('Ctrl Pts',(-149.901678691384,-80.9934460867894,
36.805273079051));
#23467=CARTESIAN_POINT('Ctrl Pts',(-149.909127380051,-80.9654260581732,
36.8314799870868));
#23468=CARTESIAN_POINT('Ctrl Pts',(-149.916327644768,-80.9383234966228,
36.8585857768089));
#23469=CARTESIAN_POINT('Ctrl Pts',(-149.922896825408,-80.9135964026004,
36.8833158160623));
#23470=CARTESIAN_POINT('Ctrl Pts',(-149.929259164437,-80.889633198716,36.9087941212802));
#23471=CARTESIAN_POINT('Ctrl Pts',(-149.935369835439,-80.8666055523405,
36.935135681796));
#23472=CARTESIAN_POINT('Ctrl Pts',(-149.935956871689,-80.8643933463222,
36.9376662469157));
#23473=CARTESIAN_POINT('Ctrl Pts',(-149.936541575423,-80.86218981226,36.9402047878343));
#23474=CARTESIAN_POINT('Ctrl Pts',(-149.937123900464,-80.8599951269442,
36.9427514122746));
#23475=CARTESIAN_POINT('Ctrl Pts',(-149.949888621083,-80.8118870379003,
36.9985741010473));
#23476=CARTESIAN_POINT('Ctrl Pts',(-149.961572072671,-80.7677918263995,
37.0585526832355));
#23477=CARTESIAN_POINT('Ctrl Pts',(-149.971367310254,-80.7307169524392,
37.1227154597912));
#23478=CARTESIAN_POINT('Ctrl Pts',(-149.975158206732,-80.7163684480826,
37.1475473683212));
#23479=CARTESIAN_POINT('Ctrl Pts',(-149.978650998302,-80.7031305919437,
37.1730908787877));
#23480=CARTESIAN_POINT('Ctrl Pts',(-149.981796037926,-80.6911891223571,
37.1992286595141));
#23481=CARTESIAN_POINT('Ctrl Pts',(-149.985757876154,-80.6761463323226,
37.2321546862971));
#23482=CARTESIAN_POINT('Ctrl Pts',(-149.989179977686,-80.6631984113665,
37.2661215533609));
#23483=CARTESIAN_POINT('Ctrl Pts',(-149.991954976261,-80.6527310533642,
37.3008958029159));
#23484=CARTESIAN_POINT('Ctrl Pts',(-149.993127423005,-80.6483085574699,
37.3155880467323));
#23485=CARTESIAN_POINT('Ctrl Pts',(-149.994184300917,-80.6443291875706,
37.33042386883));
#23486=CARTESIAN_POINT('Ctrl Pts',(-149.995117265699,-80.6408234431072,
37.3453832597703));
#23487=CARTESIAN_POINT('Ctrl Pts',(-149.997168971269,-80.6331138750977,
37.3782808206269));
#23488=CARTESIAN_POINT('Ctrl Pts',(-149.998622294847,-80.6276965661502,
37.4117792041199));
#23489=CARTESIAN_POINT('Ctrl Pts',(-149.999384955835,-80.624860626989,37.4456825897666));
#23490=CARTESIAN_POINT('Ctrl Pts',(-149.999789923498,-80.6233547630872,
37.4636850509239));
#23491=CARTESIAN_POINT('Ctrl Pts',(-150.,-80.6225774829854,37.481801403423));
#23492=CARTESIAN_POINT('Ctrl Pts',(-150.,-80.6225774829854,37.5));
#23493=CARTESIAN_POINT('Origin',(0.,0.,32.5));
#23494=CARTESIAN_POINT('Origin',(-147.5,-89.4427190999916,32.5));
#23495=CARTESIAN_POINT('Ctrl Pts',(-119.689439203101,-120.724637681159,
82.5));
#23496=CARTESIAN_POINT('Ctrl Pts',(-115.377099114166,-125.,82.5));
#23497=CARTESIAN_POINT('Ctrl Pts',(-121.449578014911,-125.,82.5));
#23498=CARTESIAN_POINT('Ctrl Pts',(-119.689439200917,-120.724637683324,
82.7056798133782));
#23499=CARTESIAN_POINT('Ctrl Pts',(-115.377099118341,-124.999999995701,
82.3507082521197));
#23500=CARTESIAN_POINT('Ctrl Pts',(-121.449578012695,-125.,82.6028399066646));
#23501=CARTESIAN_POINT('Ctrl Pts',(-119.676882557983,-120.737090180421,
82.9079954286207));
#23502=CARTESIAN_POINT('Ctrl Pts',(-115.401361881511,-124.975048941511,
82.2053610116202));
#23503=CARTESIAN_POINT('Ctrl Pts',(-121.436836713265,-125.006317811859,
82.7039977143433));
#23504=CARTESIAN_POINT('Ctrl Pts',(-119.628410587298,-120.785117230515,
83.3063417968652));
#23505=CARTESIAN_POINT('Ctrl Pts',(-115.489012547634,-124.884856124345,
81.9514922386294));
#23506=CARTESIAN_POINT('Ctrl Pts',(-121.387651919446,-125.030684477513,
82.9031708983997));
#23507=CARTESIAN_POINT('Ctrl Pts',(-119.592485604525,-120.820701126369,
83.5023756354685));
#23508=CARTESIAN_POINT('Ctrl Pts',(-115.551419916513,-124.820623886438,
81.844093442978));
#23509=CARTESIAN_POINT('Ctrl Pts',(-121.351198628156,-125.048738071447,
83.0011878177447));
#23510=CARTESIAN_POINT('Ctrl Pts',(-119.497801818693,-120.91434900059,83.8883271564993));
#23511=CARTESIAN_POINT('Ctrl Pts',(-115.697825563992,-124.669744960185,
81.6876871655071));
#23512=CARTESIAN_POINT('Ctrl Pts',(-121.255122433638,-125.096250595907,
83.1941635782393));
#23513=CARTESIAN_POINT('Ctrl Pts',(-119.439376348876,-120.972080469663,
84.0761788301475));
#23514=CARTESIAN_POINT('Ctrl Pts',(-115.779889571829,-124.585091209873,
81.639444465222));
#23515=CARTESIAN_POINT('Ctrl Pts',(-121.195837765812,-125.125540825988,
83.2880894152805));
#23516=CARTESIAN_POINT('Ctrl Pts',(-119.305221428487,-121.104388919918,
84.4342801401529));
#23517=CARTESIAN_POINT('Ctrl Pts',(-115.940258775456,-124.419250986645,
81.6056236890861));
#23518=CARTESIAN_POINT('Ctrl Pts',(-121.059709978865,-125.192667908432,
83.4671400698696));
#23519=CARTESIAN_POINT('Ctrl Pts',(-119.229146767872,-121.179307379907,
84.6059387232763));
#23520=CARTESIAN_POINT('Ctrl Pts',(-116.018662098376,-124.337976550129,
81.6177805257506));
#23521=CARTESIAN_POINT('Ctrl Pts',(-120.982516573327,-125.230678008636,
83.5529693617978));
#23522=CARTESIAN_POINT('Ctrl Pts',(-119.060491893051,-121.345017393603,
84.9357796688685));
#23523=CARTESIAN_POINT('Ctrl Pts',(-116.159254888288,-124.191486350903,
81.6927658265867));
#23524=CARTESIAN_POINT('Ctrl Pts',(-120.811381479668,-125.314751472042,
83.7178898342746));
#23525=CARTESIAN_POINT('Ctrl Pts',(-118.96776206845,-121.435951457507,85.093861858456));
#23526=CARTESIAN_POINT('Ctrl Pts',(-116.221496701314,-124.12623198531,81.7541916577615));
#23527=CARTESIAN_POINT('Ctrl Pts',(-120.717287981259,-125.36088713601,83.7969309295804));
#23528=CARTESIAN_POINT('Ctrl Pts',(-118.772148188168,-121.627281202587,
85.3899146057789));
#23529=CARTESIAN_POINT('Ctrl Pts',(-116.320002770212,-124.021697634043,
81.9095222659674));
#23530=CARTESIAN_POINT('Ctrl Pts',(-120.518797426192,-125.45795884595,83.9449573025371));
#23531=CARTESIAN_POINT('Ctrl Pts',(-118.66868983755,-121.728242289117,85.5290754975167));
#23532=CARTESIAN_POINT('Ctrl Pts',(-116.35752640374,-123.981145420879,82.0023320413466));
#23533=CARTESIAN_POINT('Ctrl Pts',(-120.413817629313,-125.50918174931,84.0145377490307));
#23534=CARTESIAN_POINT('Ctrl Pts',(-118.45169839953,-121.939403249423,85.7917547211079));
#23535=CARTESIAN_POINT('Ctrl Pts',(-116.406873166747,-123.925571355125,
82.2074570860312));
#23536=CARTESIAN_POINT('Ctrl Pts',(-120.193635140666,-125.616314884214,
84.1458773602816));
#23537=CARTESIAN_POINT('Ctrl Pts',(-118.338158476483,-122.049610026221,
85.9152619328964));
#23538=CARTESIAN_POINT('Ctrl Pts',(-116.419520677459,-123.909734352817,
82.3190059601612));
#23539=CARTESIAN_POINT('Ctrl Pts',(-120.078425512936,-125.672228616066,
84.2076309666417));
#23540=CARTESIAN_POINT('Ctrl Pts',(-118.101739972007,-122.278395780866,
86.1479296435188));
#23541=CARTESIAN_POINT('Ctrl Pts',(-116.420156575106,-123.902371131663,
82.5520650696801));
#23542=CARTESIAN_POINT('Ctrl Pts',(-119.838530265679,-125.788303741941,
84.323964821566));
#23543=CARTESIAN_POINT('Ctrl Pts',(-117.978621353548,-122.397201959151,
86.2571677342239));
#23544=CARTESIAN_POINT('Ctrl Pts',(-116.408784821067,-123.910208556756,
82.6734238697007));
#23545=CARTESIAN_POINT('Ctrl Pts',(-119.713601079353,-125.848580405477,
84.3785838674499));
#23546=CARTESIAN_POINT('Ctrl Pts',(-117.603241895162,-122.758291253176,
86.5592543593046));
#23547=CARTESIAN_POINT('Ctrl Pts',(-116.343210235511,-123.964762276173,
83.0296153459409));
#23548=CARTESIAN_POINT('Ctrl Pts',(-119.332701334762,-126.031780121634,
84.5296271789764));
#23549=CARTESIAN_POINT('Ctrl Pts',(-117.342767505456,-123.007368772318,
86.7291564746629));
#23550=CARTESIAN_POINT('Ctrl Pts',(-116.259553389397,-124.040181684855,
83.2697315003776));
#23551=CARTESIAN_POINT('Ctrl Pts',(-119.068396439392,-126.158150332831,
84.6145782376957));
#23552=CARTESIAN_POINT('Ctrl Pts',(-116.804336290701,-123.518763278367,
87.016825817368));
#23553=CARTESIAN_POINT('Ctrl Pts',(-116.02736829311,-124.252946369571,83.719666170302));
#23554=CARTESIAN_POINT('Ctrl Pts',(-118.522047118472,-126.417607839943,
84.7584129083197));
#23555=CARTESIAN_POINT('Ctrl Pts',(-116.525023660543,-123.782353191698,
87.1348755768559));
#23556=CARTESIAN_POINT('Ctrl Pts',(-115.881406957195,-124.387808755614,
83.9325453429328));
#23557=CARTESIAN_POINT('Ctrl Pts',(-118.238626949676,-126.551340957402,
84.8174377888648));
#23558=CARTESIAN_POINT('Ctrl Pts',(-115.67127235659,-124.582362934986,87.4141780079963));
#23559=CARTESIAN_POINT('Ctrl Pts',(-115.387279747809,-124.844116246409,
84.4905439734664));
#23560=CARTESIAN_POINT('Ctrl Pts',(-117.372320479466,-126.95722825408,84.9570890031244));
#23561=CARTESIAN_POINT('Ctrl Pts',(-115.09272258053,-125.11712992375,87.4999999999441));
#23562=CARTESIAN_POINT('Ctrl Pts',(-114.975356365161,-125.224084605227,
84.7914664637573));
#23563=CARTESIAN_POINT('Ctrl Pts',(-116.78526355091,-127.228543433485,85.));
#23564=CARTESIAN_POINT('Ctrl Pts',(-114.505594583524,-125.652173913043,
87.5));
#23565=CARTESIAN_POINT('Ctrl Pts',(-114.505594583524,-125.652173913043,
85.));
#23566=CARTESIAN_POINT('Ctrl Pts',(-116.189500386222,-127.5,85.));
#23567=CARTESIAN_POINT('Origin',(-121.449578014911,-122.5,82.5));
#23568=CARTESIAN_POINT('Origin',(-147.5,-122.5,44.5));
#23569=CARTESIAN_POINT('Origin',(-147.5,-122.5,49.5));
#23570=CARTESIAN_POINT('Origin',(-147.5,-122.5,44.5));
#23571=CARTESIAN_POINT('Ctrl Pts',(-145.36231884058,-88.1464478086873,32.5));
#23572=CARTESIAN_POINT('Ctrl Pts',(-145.36231884058,-88.1464478086873,35.));
#23573=CARTESIAN_POINT('Ctrl Pts',(-147.5,-89.4427190999916,35.));
#23574=CARTESIAN_POINT('Ctrl Pts',(-145.88328041902,-87.2873300001825,32.5000000009303));
#23575=CARTESIAN_POINT('Ctrl Pts',(-145.793011707092,-87.4361921450511,
34.7836438007663));
#23576=CARTESIAN_POINT('Ctrl Pts',(-147.764311380887,-88.5709672327986,
35.));
#23577=CARTESIAN_POINT('Ctrl Pts',(-146.390924783419,-86.432995377738,32.5817470282981));
#23578=CARTESIAN_POINT('Ctrl Pts',(-146.25636627112,-86.6602829701382,34.6533815799931));
#23579=CARTESIAN_POINT('Ctrl Pts',(-148.021866250329,-87.7040688391623,
35.0408735143651));
#23580=CARTESIAN_POINT('Ctrl Pts',(-147.13295559207,-85.1594666843921,32.8264997589536));
#23581=CARTESIAN_POINT('Ctrl Pts',(-146.95625485105,-85.4644664729224,34.606035054135));
#23582=CARTESIAN_POINT('Ctrl Pts',(-148.398337763665,-86.4118117826985,
35.1632498793688));
#23583=CARTESIAN_POINT('Ctrl Pts',(-147.377049426154,-84.7363019818542,
32.9287776457782));
#23584=CARTESIAN_POINT('Ctrl Pts',(-147.185340564392,-85.0695699101127,
34.6128471107274));
#23585=CARTESIAN_POINT('Ctrl Pts',(-148.522179488132,-85.9824240698147,
35.2143888231312));
#23586=CARTESIAN_POINT('Ctrl Pts',(-147.858493843555,-83.8933928830767,
33.1802802395072));
#23587=CARTESIAN_POINT('Ctrl Pts',(-147.640340054158,-84.2776371924663,
34.6763398436954));
#23588=CARTESIAN_POINT('Ctrl Pts',(-148.766441729588,-85.1271192490123,
35.3401401195115));
#23589=CARTESIAN_POINT('Ctrl Pts',(-148.095887496716,-83.4735259621086,
33.329690382783));
#23590=CARTESIAN_POINT('Ctrl Pts',(-147.866955151253,-83.8795640251351,
34.7317798844392));
#23591=CARTESIAN_POINT('Ctrl Pts',(-148.886884097334,-84.7010778144719,
35.4148451917151));
#23592=CARTESIAN_POINT('Ctrl Pts',(-148.555727425865,-82.65238822296,33.6809331684156));
#23593=CARTESIAN_POINT('Ctrl Pts',(-148.307824862021,-83.0977615436487,
34.8965208417471));
#23594=CARTESIAN_POINT('Ctrl Pts',(-149.120185238387,-83.867864520377,35.5904665838843));
#23595=CARTESIAN_POINT('Ctrl Pts',(-148.780093861296,-82.2476812683581,
33.8839399244617));
#23596=CARTESIAN_POINT('Ctrl Pts',(-148.524727773055,-82.7095240936236,
35.0050364952365));
#23597=CARTESIAN_POINT('Ctrl Pts',(-149.234018208522,-83.457205992854,35.691969962678));
#23598=CARTESIAN_POINT('Ctrl Pts',(-149.207972890121,-81.4688789012013,
34.3573989375128));
#23599=CARTESIAN_POINT('Ctrl Pts',(-148.93931728545,-81.9607628458225,35.2860875789467));
#23600=CARTESIAN_POINT('Ctrl Pts',(-149.4511038933,-82.6669506497871,35.9286994683092));
#23601=CARTESIAN_POINT('Ctrl Pts',(-149.410469407752,-81.0966396786721,
34.6254381321728));
#23602=CARTESIAN_POINT('Ctrl Pts',(-149.13707735126,-81.6002642788733,35.4559386647908));
#23603=CARTESIAN_POINT('Ctrl Pts',(-149.553841095111,-82.2892373209608,
36.0627190669335));
#23604=CARTESIAN_POINT('Ctrl Pts',(-149.689478100498,-80.5797647052593,
35.1010485304976));
#23605=CARTESIAN_POINT('Ctrl Pts',(-149.410828634125,-81.0973762069276,
35.7764659917703));
#23606=CARTESIAN_POINT('Ctrl Pts',(-149.695396978193,-81.7647612450649,
36.3005242648253));
#23607=CARTESIAN_POINT('Ctrl Pts',(-149.778860900691,-80.4134491496535,
35.2734504935396));
#23608=CARTESIAN_POINT('Ctrl Pts',(-149.498351131341,-80.935915280146,35.8944893614103));
#23609=CARTESIAN_POINT('Ctrl Pts',(-149.74074560314,-81.5959998724055,36.3867252471529));
#23610=CARTESIAN_POINT('Ctrl Pts',(-149.942345818684,-80.1081950067706,
35.6444293836573));
#23611=CARTESIAN_POINT('Ctrl Pts',(-149.658443692203,-80.6395711160542,
36.1532547010742));
#23612=CARTESIAN_POINT('Ctrl Pts',(-149.823690158896,-81.2862566980837,
36.5722146914456));
#23613=CARTESIAN_POINT('Ctrl Pts',(-150.016754772459,-79.9686937648418,
35.8430315532085));
#23614=CARTESIAN_POINT('Ctrl Pts',(-149.731542660712,-80.5037270542566,
36.2939840338164));
#23615=CARTESIAN_POINT('Ctrl Pts',(-149.861441758745,-81.144703967216,36.6715157768338));
#23616=CARTESIAN_POINT('Ctrl Pts',(-150.145196691125,-79.7272764209246,
36.2762826327136));
#23617=CARTESIAN_POINT('Ctrl Pts',(-149.857607243134,-80.2688649285009,
36.6048325581329));
#23618=CARTESIAN_POINT('Ctrl Pts',(-149.926607145573,-80.8997363683411,
36.8881413161273));
#23619=CARTESIAN_POINT('Ctrl Pts',(-150.197080555724,-79.6294105444985,
36.5038809199123));
#23620=CARTESIAN_POINT('Ctrl Pts',(-149.908727602392,-80.1732994372084,
36.7701162187303));
#23621=CARTESIAN_POINT('Ctrl Pts',(-149.952930574586,-80.8004312877628,
37.0019404601773));
#23622=CARTESIAN_POINT('Ctrl Pts',(-150.269771338359,-79.4921496315481,
36.9870649844503));
#23623=CARTESIAN_POINT('Ctrl Pts',(-149.980179574577,-80.0395829024242,
37.1229099719677));
#23624=CARTESIAN_POINT('Ctrl Pts',(-149.989810459912,-80.6611518320492,
37.243532492004));
#23625=CARTESIAN_POINT('Ctrl Pts',(-150.289855071895,-79.4541343321333,
37.2465705504854));
#23626=CARTESIAN_POINT('Ctrl Pts',(-149.99999999943,-80.0024038110911,37.313811727788));
#23627=CARTESIAN_POINT('Ctrl Pts',(-150.,-80.6225774840775,37.3732852754135));
#23628=CARTESIAN_POINT('Ctrl Pts',(-150.289855072464,-79.4541343310581,
37.5));
#23629=CARTESIAN_POINT('Ctrl Pts',(-150.,-80.0024038100394,37.5));
#23630=CARTESIAN_POINT('Ctrl Pts',(-150.,-80.6225774829855,37.5));
#23631=CARTESIAN_POINT('Origin',(-152.5,-80.6225774829854,37.5));
#23632=CARTESIAN_POINT('Origin',(-121.449578014911,-122.5,115.));
#23633=CARTESIAN_POINT('Origin',(-115.217186218029,-122.5,49.5));
#23634=CARTESIAN_POINT('Origin',(-147.5,0.,44.5));
#23635=CARTESIAN_POINT('Ctrl Pts',(-150.,-80.6225774829854,44.5));
#23636=CARTESIAN_POINT('Ctrl Pts',(-150.,-80.6225774829854,44.5312343888304));
#23637=CARTESIAN_POINT('Ctrl Pts',(-149.999418286665,-80.6247797743348,
44.5621210164789));
#23638=CARTESIAN_POINT('Ctrl Pts',(-149.998293554945,-80.6290354954265,
44.5925723355625));
#23639=CARTESIAN_POINT('Ctrl Pts',(-149.997125538082,-80.6334549973542,
44.6241955694378));
#23640=CARTESIAN_POINT('Ctrl Pts',(-149.995371936956,-80.6400888791781,
44.655349356458));
#23641=CARTESIAN_POINT('Ctrl Pts',(-149.993090530187,-80.6487160556979,
44.6859412124329));
#23642=CARTESIAN_POINT('Ctrl Pts',(-149.992231155702,-80.6519657941861,
44.6974647429366));
#23643=CARTESIAN_POINT('Ctrl Pts',(-149.991297028852,-80.6554978429527,
44.7089085934095));
#23644=CARTESIAN_POINT('Ctrl Pts',(-149.990291719683,-80.6592985775913,
44.7202680068894));
#23645=CARTESIAN_POINT('Ctrl Pts',(-149.987499102739,-80.6698565196466,
44.7518229668389));
#23646=CARTESIAN_POINT('Ctrl Pts',(-149.984157100677,-80.6824881297728,
44.7827141728588));
#23647=CARTESIAN_POINT('Ctrl Pts',(-149.980355786964,-80.6968505802923,
44.8128256266941));
#23648=CARTESIAN_POINT('Ctrl Pts',(-149.977558137322,-80.7074209008703,
44.8349867279405));
#23649=CARTESIAN_POINT('Ctrl Pts',(-149.974509955706,-80.7189351701335,
44.8567449506927));
#23650=CARTESIAN_POINT('Ctrl Pts',(-149.971243495187,-80.7312708109915,
44.8780946805967));
#23651=CARTESIAN_POINT('Ctrl Pts',(-149.965898079908,-80.7514575307578,
44.9130325504344));
#23652=CARTESIAN_POINT('Ctrl Pts',(-149.960009186179,-80.773686648641,44.9465704967713));
#23653=CARTESIAN_POINT('Ctrl Pts',(-149.953740444404,-80.797335293561,44.9787015735967));
#23654=CARTESIAN_POINT('Ctrl Pts',(-149.948225014278,-80.8181420923231,
45.0069714745479));
#23655=CARTESIAN_POINT('Ctrl Pts',(-149.9424154207,-80.8400482470994,45.0341525202745));
#23656=CARTESIAN_POINT('Ctrl Pts',(-149.936415096464,-80.8626613647233,
45.0602466352771));
#23657=CARTESIAN_POINT('Ctrl Pts',(-149.930229230798,-80.8859737229195,
45.0871476299065));
#23658=CARTESIAN_POINT('Ctrl Pts',(-149.923781601043,-80.9102578633712,
45.1131530185116));
#23659=CARTESIAN_POINT('Ctrl Pts',(-149.917129634266,-80.9352949903539,
45.1383421170535));
#23660=CARTESIAN_POINT('Ctrl Pts',(-149.910169623638,-80.9614915538295,
45.1646976896917));
#23661=CARTESIAN_POINT('Ctrl Pts',(-149.902985851619,-80.9885126935503,
45.1901596664586));
#23662=CARTESIAN_POINT('Ctrl Pts',(-149.895629953764,-81.0161619977713,
45.2148125956205));
#23663=CARTESIAN_POINT('Ctrl Pts',(-149.894768894784,-81.0193985410376,
45.2176983923565));
#23664=CARTESIAN_POINT('Ctrl Pts',(-149.893905462669,-81.0226437475977,
45.2205730959881));
#23665=CARTESIAN_POINT('Ctrl Pts',(-149.893039728921,-81.0258973457795,
45.2234368363464));
#23666=CARTESIAN_POINT('Ctrl Pts',(-149.885294621979,-81.055004985282,45.2490566939069));
#23667=CARTESIAN_POINT('Ctrl Pts',(-149.877335285324,-81.0848961910411,
45.2738874208924));
#23668=CARTESIAN_POINT('Ctrl Pts',(-149.869211724912,-81.1153826082176,
45.2979942587922));
#23669=CARTESIAN_POINT('Ctrl Pts',(-149.860756318493,-81.1471143901477,
45.3230858567598));
#23670=CARTESIAN_POINT('Ctrl Pts',(-149.852122887,-81.179491428094,45.3473933229362));
#23671=CARTESIAN_POINT('Ctrl Pts',(-149.843353240441,-81.212356779593,45.3709861423032));
#23672=CARTESIAN_POINT('Ctrl Pts',(-149.834033859779,-81.2472823286657,
45.3960579012523));
#23673=CARTESIAN_POINT('Ctrl Pts',(-149.824560562659,-81.282759673792,45.420322766943));
#23674=CARTESIAN_POINT('Ctrl Pts',(-149.814968902639,-81.318656015993,45.4438574826091));
#23675=CARTESIAN_POINT('Ctrl Pts',(-149.814245534136,-81.3213631890219,
45.4456323862228));
#23676=CARTESIAN_POINT('Ctrl Pts',(-149.813521486337,-81.3240727682655,
45.4474031333746));
#23677=CARTESIAN_POINT('Ctrl Pts',(-149.81279677161,-81.3267847076918,45.4491697551619));
#23678=CARTESIAN_POINT('Ctrl Pts',(-149.802161746897,-81.3665818053887,
45.4750945303171));
#23679=CARTESIAN_POINT('Ctrl Pts',(-149.791378236576,-81.4068954418303,
45.5001449499175));
#23680=CARTESIAN_POINT('Ctrl Pts',(-149.780505488345,-81.4474999785173,
45.5243508763432));
#23681=CARTESIAN_POINT('Ctrl Pts',(-149.766212096436,-81.5008789903218,
45.5561721588362));
#23682=CARTESIAN_POINT('Ctrl Pts',(-149.75173104415,-81.5548874755347,45.5866585651915));
#23683=CARTESIAN_POINT('Ctrl Pts',(-149.7370901728,-81.6094178533078,45.6160154789332));
#23684=CARTESIAN_POINT('Ctrl Pts',(-149.721679195218,-81.6668165155371,
45.6469165591158));
#23685=CARTESIAN_POINT('Ctrl Pts',(-149.706091100881,-81.7247936014321,
45.6765660851853));
#23686=CARTESIAN_POINT('Ctrl Pts',(-149.690345642873,-81.7832715016962,
45.7051731327433));
#23687=CARTESIAN_POINT('Ctrl Pts',(-149.684002656688,-81.8068290579963,
45.7166973518138));
#23688=CARTESIAN_POINT('Ctrl Pts',(-149.67763399788,-81.8304683944407,45.7280520707485));
#23689=CARTESIAN_POINT('Ctrl Pts',(-149.671240444102,-81.854186356593,45.7392497349255));
#23690=CARTESIAN_POINT('Ctrl Pts',(-149.663115656512,-81.8843266214971,
45.7534794803999));
#23691=CARTESIAN_POINT('Ctrl Pts',(-149.654955183208,-81.9145791058626,
45.7674477491405));
#23692=CARTESIAN_POINT('Ctrl Pts',(-149.646761444289,-81.9449339838539,
45.7811773107384));
#23693=CARTESIAN_POINT('Ctrl Pts',(-149.629599044989,-82.0085145472401,
45.8099349048783));
#23694=CARTESIAN_POINT('Ctrl Pts',(-149.612256027528,-82.0726719053374,
45.8376821506386));
#23695=CARTESIAN_POINT('Ctrl Pts',(-149.594776281623,-82.1372383448953,
45.8645156723128));
#23696=CARTESIAN_POINT('Ctrl Pts',(-149.57592605508,-82.2068670465535,45.8934530473311));
#23697=CARTESIAN_POINT('Ctrl Pts',(-149.556916727547,-82.2769718987423,
45.9213279816653));
#23698=CARTESIAN_POINT('Ctrl Pts',(-149.537787182918,-82.3473991049663,
45.9482460618992));
#23699=CARTESIAN_POINT('Ctrl Pts',(-149.532245072383,-82.3678029028159,
45.9560446257929));
#23700=CARTESIAN_POINT('Ctrl Pts',(-149.526692780135,-82.3882340721267,
45.9637627732937));
#23701=CARTESIAN_POINT('Ctrl Pts',(-149.521131044556,-82.4086895813368,
45.9714028195526));
#23702=CARTESIAN_POINT('Ctrl Pts',(-149.513307047732,-82.4374654619684,
45.9821504893812));
#23703=CARTESIAN_POINT('Ctrl Pts',(-149.505462657808,-82.4662967316413,
45.9927459306726));
#23704=CARTESIAN_POINT('Ctrl Pts',(-149.497602582526,-82.4951656239004,
46.0031912460791));
#23705=CARTESIAN_POINT('Ctrl Pts',(-149.466886299739,-82.6079819808148,
46.0440103540796));
#23706=CARTESIAN_POINT('Ctrl Pts',(-149.435949796432,-82.721306238521,46.0825462658463));
#23707=CARTESIAN_POINT('Ctrl Pts',(-149.404819096531,-82.8350358342389,
46.1191658716245));
#23708=CARTESIAN_POINT('Ctrl Pts',(-149.382928718768,-82.9150078175565,
46.1449159192168));
#23709=CARTESIAN_POINT('Ctrl Pts',(-149.360942099001,-82.995181007926,46.169717455523));
#23710=CARTESIAN_POINT('Ctrl Pts',(-149.338865605393,-83.0755291035976,
46.193686300737));
#23711=CARTESIAN_POINT('Ctrl Pts',(-149.30257270251,-83.2076182697843,46.233090156576));
#23712=CARTESIAN_POINT('Ctrl Pts',(-149.266041574139,-83.3401623692395,
46.2702654172594));
#23713=CARTESIAN_POINT('Ctrl Pts',(-149.229255373738,-83.4732146574125,
46.3055170512346));
#23714=CARTESIAN_POINT('Ctrl Pts',(-149.222100057115,-83.4990947765572,
46.3123738779743));
#23715=CARTESIAN_POINT('Ctrl Pts',(-149.214935059986,-83.5249942184406,
46.3191578024711));
#23716=CARTESIAN_POINT('Ctrl Pts',(-149.207760216038,-83.5509135089673,
46.3258708967128));
#23717=CARTESIAN_POINT('Ctrl Pts',(-149.164019348336,-83.7089284102155,
46.366796743915));
#23718=CARTESIAN_POINT('Ctrl Pts',(-149.119950314816,-83.8675446159544,
46.4050588777709));
#23719=CARTESIAN_POINT('Ctrl Pts',(-149.075578120339,-84.0266555943282,
46.4410493230434));
#23720=CARTESIAN_POINT('Ctrl Pts',(-149.050851325548,-84.1153215834145,
46.4611053145304));
#23721=CARTESIAN_POINT('Ctrl Pts',(-149.026030206988,-84.2041418314762,
46.4804550867179));
#23722=CARTESIAN_POINT('Ctrl Pts',(-149.001117827171,-84.2931021083258,
46.4991611413161));
#23723=CARTESIAN_POINT('Ctrl Pts',(-148.961812515426,-84.4334584869728,
46.5286744721549));
#23724=CARTESIAN_POINT('Ctrl Pts',(-148.922228706232,-84.5743409203763,
46.5565824640166));
#23725=CARTESIAN_POINT('Ctrl Pts',(-148.882458149795,-84.7154243069172,
46.58297626425));
#23726=CARTESIAN_POINT('Ctrl Pts',(-148.823378480021,-84.9250054803839,
46.6221845917561));
#23727=CARTESIAN_POINT('Ctrl Pts',(-148.763691428381,-85.1357176965639,
46.658180607518));
#23728=CARTESIAN_POINT('Ctrl Pts',(-148.703725142332,-85.346373256235,46.6911268937745));
#23729=CARTESIAN_POINT('Ctrl Pts',(-148.683093735236,-85.4188493239555,
46.7024620670668));
#23730=CARTESIAN_POINT('Ctrl Pts',(-148.662429146923,-85.4913191022908,
46.7134360383522));
#23731=CARTESIAN_POINT('Ctrl Pts',(-148.64174438629,-85.5637353575988,46.7240548006858));
#23732=CARTESIAN_POINT('Ctrl Pts',(-148.565624143843,-85.8302283090543,
46.7631320120529));
#23733=CARTESIAN_POINT('Ctrl Pts',(-148.489028565031,-86.0967324995911,
46.7975654258511));
#23734=CARTESIAN_POINT('Ctrl Pts',(-148.411875341988,-86.3635238183437,
46.8277812265461));
#23735=CARTESIAN_POINT('Ctrl Pts',(-148.365096720961,-86.5252815453832,
46.846101310063));
#23736=CARTESIAN_POINT('Ctrl Pts',(-148.318112978006,-86.6871449972432,
46.8628698580675));
#23737=CARTESIAN_POINT('Ctrl Pts',(-148.270904619886,-86.8491769961467,
46.8781728422293));
#23738=CARTESIAN_POINT('Ctrl Pts',(-148.24918654488,-86.9237193705385,46.8852129379044));
#23739=CARTESIAN_POINT('Ctrl Pts',(-148.227421070419,-86.9982969676292,
46.8919477958447));
#23740=CARTESIAN_POINT('Ctrl Pts',(-148.205605817643,-87.0729174681581,
46.8983780579096));
#23741=CARTESIAN_POINT('Ctrl Pts',(-148.10190068443,-87.42764766667,46.9289461742125));
#23742=CARTESIAN_POINT('Ctrl Pts',(-147.997167488693,-87.7829762387816,
46.9525973445083));
#23743=CARTESIAN_POINT('Ctrl Pts',(-147.891499227195,-88.1385323929249,
46.969351029831));
#23744=CARTESIAN_POINT('Ctrl Pts',(-147.785745335364,-88.4943766789206,
46.9861182918287));
#23745=CARTESIAN_POINT('Ctrl Pts',(-147.679054863979,-88.8504488649393,
46.9959768816863));
#23746=CARTESIAN_POINT('Ctrl Pts',(-147.571529965735,-89.2063722196095,
46.9989975290796));
#23747=CARTESIAN_POINT('Ctrl Pts',(-147.547727111398,-89.285163196442,46.9996662116924));
#23748=CARTESIAN_POINT('Ctrl Pts',(-147.523883400528,-89.3639468619846,
47.));
#23749=CARTESIAN_POINT('Ctrl Pts',(-147.5,-89.4427190999916,47.));
#23750=CARTESIAN_POINT('Origin',(-152.5,-80.6225774829854,115.));
#23751=CARTESIAN_POINT('Origin',(-152.5,-80.6225774829854,44.5));
#23752=CARTESIAN_POINT('Ctrl Pts',(-150.289855072464,-79.4541343310581,
44.5));
#23753=CARTESIAN_POINT('Ctrl Pts',(-150.,-80.0024038100394,44.5));
#23754=CARTESIAN_POINT('Ctrl Pts',(-150.,-80.6225774829855,44.5));
#23755=CARTESIAN_POINT('Ctrl Pts',(-150.28985506853,-79.4541343384987,44.7594238560556));
#23756=CARTESIAN_POINT('Ctrl Pts',(-149.999999996126,-80.0024038172978,
44.6905851824362));
#23757=CARTESIAN_POINT('Ctrl Pts',(-150.,-80.6225774905387,44.629711927975));
#23758=CARTESIAN_POINT('Ctrl Pts',(-150.270119749701,-79.4914922605508,
45.0111695802387));
#23759=CARTESIAN_POINT('Ctrl Pts',(-149.980519833119,-80.0389466368966,
44.8758156770736));
#23760=CARTESIAN_POINT('Ctrl Pts',(-149.989987226484,-80.6604847938369,
44.7555847901951));
#23761=CARTESIAN_POINT('Ctrl Pts',(-150.196231486305,-79.6310132970258,
45.5012087006257));
#23762=CARTESIAN_POINT('Ctrl Pts',(-149.907890955038,-80.1748646486434,
45.2336047942099));
#23763=CARTESIAN_POINT('Ctrl Pts',(-149.952499797667,-80.8020576101747,
45.0006043502371));
#23764=CARTESIAN_POINT('Ctrl Pts',(-150.143050717941,-79.7313168859281,
45.7320003431406));
#23765=CARTESIAN_POINT('Ctrl Pts',(-149.855501091412,-80.272795283317,45.4011397919881));
#23766=CARTESIAN_POINT('Ctrl Pts',(-149.925518380098,-80.9038362519448,
45.1160001719023));
#23767=CARTESIAN_POINT('Ctrl Pts',(-150.01502846971,-79.971931353987,46.1617150079383));
#23768=CARTESIAN_POINT('Ctrl Pts',(-149.729850869406,-80.506872138187,45.7093793927994));
#23769=CARTESIAN_POINT('Ctrl Pts',(-149.860565913637,-81.1479891679691,
45.3308575036371));
#23770=CARTESIAN_POINT('Ctrl Pts',(-149.939105635844,-80.1142600764838,
46.3637363656926));
#23771=CARTESIAN_POINT('Ctrl Pts',(-149.655266820466,-80.6454659182033,
45.8524984192499));
#23772=CARTESIAN_POINT('Ctrl Pts',(-149.8220462428,-81.2924109599909,45.4318681833206));
#23773=CARTESIAN_POINT('Ctrl Pts',(-149.775363670977,-80.4199633406152,
46.7336380224264));
#23774=CARTESIAN_POINT('Ctrl Pts',(-149.494928348598,-80.9422362487695,
46.1103934277676));
#23775=CARTESIAN_POINT('Ctrl Pts',(-149.738971273161,-81.6026098603007,
45.616819010739));
#23776=CARTESIAN_POINT('Ctrl Pts',(-149.686995608736,-80.5843780010491,
46.903585266663));
#23777=CARTESIAN_POINT('Ctrl Pts',(-149.408398325687,-81.1018541496878,
46.2266925752405));
#23778=CARTESIAN_POINT('Ctrl Pts',(-149.694137478568,-81.7694423834459,
45.7017926336777));
#23779=CARTESIAN_POINT('Ctrl Pts',(-149.500255462679,-80.9302925286903,
47.2210941330543));
#23780=CARTESIAN_POINT('Ctrl Pts',(-149.226078269656,-81.4367533718067,
46.4395269094013));
#23781=CARTESIAN_POINT('Ctrl Pts',(-149.599394315017,-82.1204438893779,
45.8605470661809));
#23782=CARTESIAN_POINT('Ctrl Pts',(-149.401347886678,-81.1127763961003,
47.369210707149));
#23783=CARTESIAN_POINT('Ctrl Pts',(-149.129574349821,-81.6133256610688,
46.5363235480013));
#23784=CARTESIAN_POINT('Ctrl Pts',(-149.549213266548,-82.3056113431187,
45.9346053539496));
#23785=CARTESIAN_POINT('Ctrl Pts',(-149.197899201605,-81.4863922312653,
47.6435514113241));
#23786=CARTESIAN_POINT('Ctrl Pts',(-148.93165319989,-81.9738530462045,46.7107456147876));
#23787=CARTESIAN_POINT('Ctrl Pts',(-149.445992976772,-82.684721528767,46.071775705287));
#23788=CARTESIAN_POINT('Ctrl Pts',(-149.093462145135,-81.6773447374821,
47.7698090460946));
#23789=CARTESIAN_POINT('Ctrl Pts',(-148.830186520417,-82.1578926315274,
46.7883037911384));
#23790=CARTESIAN_POINT('Ctrl Pts',(-149.393006529828,-82.8784821601051,
46.1349045233201));
#23791=CARTESIAN_POINT('Ctrl Pts',(-148.773324875584,-82.2599185303359,
48.1224993059861));
#23792=CARTESIAN_POINT('Ctrl Pts',(-148.518202139789,-82.721231742148,46.9985052310704));
#23793=CARTESIAN_POINT('Ctrl Pts',(-149.230583943609,-83.4696232145796,
46.3112496524474));
#23794=CARTESIAN_POINT('Ctrl Pts',(-148.550873607932,-82.6611103319713,
48.3232112727545));
#23795=CARTESIAN_POINT('Ctrl Pts',(-148.30315471628,-83.1060920248234,47.1056075630378));
#23796=CARTESIAN_POINT('Ctrl Pts',(-149.117722639557,-83.8767148956951,
46.4116056366651));
#23797=CARTESIAN_POINT('Ctrl Pts',(-148.091214058598,-83.4818155626998,
48.6734332925097));
#23798=CARTESIAN_POINT('Ctrl Pts',(-147.862495369544,-83.8874214153556,
47.2694844772005));
#23799=CARTESIAN_POINT('Ctrl Pts',(-148.884513014786,-84.7094893209564,
46.586716645967));
#23800=CARTESIAN_POINT('Ctrl Pts',(-147.853104568995,-83.9028862659541,
48.8228865658125));
#23801=CARTESIAN_POINT('Ctrl Pts',(-147.635229789707,-84.286581928446,47.3247069198698));
#23802=CARTESIAN_POINT('Ctrl Pts',(-148.763707465283,-85.1367522404598,
46.6614432831528));
#23803=CARTESIAN_POINT('Ctrl Pts',(-147.37234266623,-84.7444834282146,49.073322172108));
#23804=CARTESIAN_POINT('Ctrl Pts',(-147.180928816256,-85.0771956930355,
47.3874171310308));
#23805=CARTESIAN_POINT('Ctrl Pts',(-148.519791499647,-85.9907258315643,
46.7866610858075));
#23806=CARTESIAN_POINT('Ctrl Pts',(-147.128665473946,-85.166872640511,49.1751382031672));
#23807=CARTESIAN_POINT('Ctrl Pts',(-146.952267516978,-85.4713149459694,
47.3939268980417));
#23808=CARTESIAN_POINT('Ctrl Pts',(-148.396161159612,-86.4193266499342,
46.837569101695));
#23809=CARTESIAN_POINT('Ctrl Pts',(-146.388097896077,-86.4377602232181,
49.41873440213));
#23810=CARTESIAN_POINT('Ctrl Pts',(-146.253862108763,-86.6644852388405,
47.3459550909554));
#23811=CARTESIAN_POINT('Ctrl Pts',(-148.020432020732,-87.7089037559046,
46.9593672008422));
#23812=CARTESIAN_POINT('Ctrl Pts',(-145.881711078451,-87.289917999924,49.4999999990937));
#23813=CARTESIAN_POINT('Ctrl Pts',(-145.791767290438,-87.4382443129923,
47.2157310733627));
#23814=CARTESIAN_POINT('Ctrl Pts',(-147.763515165397,-88.573593311031,47.));
#23815=CARTESIAN_POINT('Ctrl Pts',(-145.36231884058,-88.1464478086874,49.5));
#23816=CARTESIAN_POINT('Ctrl Pts',(-145.36231884058,-88.1464478086874,46.9999999999999));
#23817=CARTESIAN_POINT('Ctrl Pts',(-147.5,-89.4427190999917,47.));
#23818=CARTESIAN_POINT('Origin',(-147.5,-89.4427190999916,49.5));
#23819=CARTESIAN_POINT('Origin',(0.,0.,49.5));
#23820=CARTESIAN_POINT('Origin',(177.5,-137.5,-73.9644660940671));
#23821=CARTESIAN_POINT('Origin',(177.5,-137.5,-73.9644660940671));
#23822=CARTESIAN_POINT('Origin',(177.5,-137.5,-73.9644660940672));
#23823=CARTESIAN_POINT('Origin',(177.5,-137.5,-73.9644660940672));
#23824=CARTESIAN_POINT('Origin',(225.840826156048,-127.5,-25.623639938019));
#23825=CARTESIAN_POINT('Origin',(177.5,-127.5,-73.9644660940672));
#23826=CARTESIAN_POINT('Origin',(168.964466094067,-127.5,-82.5));
#23827=CARTESIAN_POINT('Origin',(177.5,-125.,-73.9644660940672));
#23828=CARTESIAN_POINT('Origin',(177.5,-127.5,-73.9644660940672));
#23829=CARTESIAN_POINT('Origin',(177.5,-137.5,85.));
#23830=CARTESIAN_POINT('Origin',(177.5,-137.5,73.9644660940673));
#23831=CARTESIAN_POINT('Origin',(258.232233047034,-137.5,6.76776695296642));
#23832=CARTESIAN_POINT('Origin',(168.964466094067,-137.5,-82.5));
#23833=CARTESIAN_POINT('Origin',(168.964466094067,0.,-82.5));
#23834=CARTESIAN_POINT('Origin',(168.964466094067,-127.5,-82.5));
#23835=CARTESIAN_POINT('Origin',(168.964466094067,-137.5,-82.5));
#23836=CARTESIAN_POINT('Origin',(168.964466094067,-127.5,-82.5));
#23837=CARTESIAN_POINT('Origin',(168.964466094067,-127.5,-82.5));
#23838=CARTESIAN_POINT('Origin',(177.5,-127.5,-73.9644660940671));
#23839=CARTESIAN_POINT('Origin',(177.5,-127.5,-73.9644660940672));
#23840=CARTESIAN_POINT('Origin',(177.5,-137.5,73.9644660940673));
#23841=CARTESIAN_POINT('Origin',(177.5,-137.5,73.9644660940673));
#23842=CARTESIAN_POINT('Origin',(177.5,-137.5,73.9644660940673));
#23843=CARTESIAN_POINT('Origin',(168.964466094067,-137.5,-82.5));
#23844=CARTESIAN_POINT('Origin',(168.964466094067,-137.5,-82.5));
#23845=CARTESIAN_POINT('Origin',(0.,-127.5,-82.5));
#23846=CARTESIAN_POINT('Ctrl Pts',(121.449578014911,-125.,-82.5));
#23847=CARTESIAN_POINT('Ctrl Pts',(121.449578013665,-125.,-82.5578430303792));
#23848=CARTESIAN_POINT('Ctrl Pts',(121.445542821646,-125.002000739817,-82.6149744276235));
#23849=CARTESIAN_POINT('Ctrl Pts',(121.437730668305,-125.005872173715,-82.6713216462809));
#23850=CARTESIAN_POINT('Ctrl Pts',(121.431548654752,-125.008935766528,-82.7159110513097));
#23851=CARTESIAN_POINT('Ctrl Pts',(121.423002583493,-125.013170255242,-82.7600095425404));
#23852=CARTESIAN_POINT('Ctrl Pts',(121.412240896123,-125.018501093781,-82.8035838902947));
#23853=CARTESIAN_POINT('Ctrl Pts',(121.402625881463,-125.023263924083,-82.8425153308796));
#23854=CARTESIAN_POINT('Ctrl Pts',(121.391240873519,-125.02890257476,-82.8810286286793));
#23855=CARTESIAN_POINT('Ctrl Pts',(121.378166904503,-125.035375090082,-82.9190974411551));
#23856=CARTESIAN_POINT('Ctrl Pts',(121.359482649641,-125.044625083389,-82.9735022966163));
#23857=CARTESIAN_POINT('Ctrl Pts',(121.337601423089,-125.055455126064,-83.0262941391226));
#23858=CARTESIAN_POINT('Ctrl Pts',(121.312984159938,-125.067631742438,-83.0775690600158));
#23859=CARTESIAN_POINT('Ctrl Pts',(121.309754155106,-125.069229423281,-83.0842967876764));
#23860=CARTESIAN_POINT('Ctrl Pts',(121.306476982697,-125.070850319854,-83.0909983906632));
#23861=CARTESIAN_POINT('Ctrl Pts',(121.303153626062,-125.072493934659,-83.0976740773907));
#23862=CARTESIAN_POINT('Ctrl Pts',(121.28333698938,-125.082294543202,-83.1374801147826));
#23863=CARTESIAN_POINT('Ctrl Pts',(121.26193952168,-125.092872330006,-83.1761870718699));
#23864=CARTESIAN_POINT('Ctrl Pts',(121.239293756531,-125.104060083144,-83.2137354525193));
#23865=CARTESIAN_POINT('Ctrl Pts',(121.223112895711,-125.112053960817,-83.2405645358963));
#23866=CARTESIAN_POINT('Ctrl Pts',(121.206293748506,-125.120359745354,-83.2668025986261));
#23867=CARTESIAN_POINT('Ctrl Pts',(121.188944294236,-125.128923152136,-83.2924342403753));
#23868=CARTESIAN_POINT('Ctrl Pts',(121.169248714547,-125.138644568041,-83.3215319880497));
#23869=CARTESIAN_POINT('Ctrl Pts',(121.148816846868,-125.14872481678,-83.3499289055538));
#23870=CARTESIAN_POINT('Ctrl Pts',(121.127768696513,-125.159103720469,-83.3776130175157));
#23871=CARTESIAN_POINT('Ctrl Pts',(121.095198113589,-125.175164368915,-83.4204523002619));
#23872=CARTESIAN_POINT('Ctrl Pts',(121.061072412821,-125.191979398504,-83.4617485539168));
#23873=CARTESIAN_POINT('Ctrl Pts',(121.025604781293,-125.209440222843,-83.5016773345161));
#23874=CARTESIAN_POINT('Ctrl Pts',(120.994690465974,-125.224659435574,-83.5364800788934));
#23875=CARTESIAN_POINT('Ctrl Pts',(120.962755773204,-125.240369726302,-83.5702435568605));
#23876=CARTESIAN_POINT('Ctrl Pts',(120.929914941896,-125.256512858459,-83.6030728931431));
#23877=CARTESIAN_POINT('Ctrl Pts',(120.919024936224,-125.261865914206,-83.6139590870702));
#23878=CARTESIAN_POINT('Ctrl Pts',(120.908034223584,-125.267267022157,-83.6247432148631));
#23879=CARTESIAN_POINT('Ctrl Pts',(120.896946618515,-125.272714234811,-83.6354286063845));
#23880=CARTESIAN_POINT('Ctrl Pts',(120.861818540488,-125.289972254912,-83.6692823795651));
#23881=CARTESIAN_POINT('Ctrl Pts',(120.825696080647,-125.307703371905,-83.7021357945807));
#23882=CARTESIAN_POINT('Ctrl Pts',(120.788855644392,-125.325770196085,-83.7339645608892));
#23883=CARTESIAN_POINT('Ctrl Pts',(120.750104876467,-125.344773861135,-83.7674437826887));
#23884=CARTESIAN_POINT('Ctrl Pts',(120.710559563373,-125.364149043197,-83.7997894992637));
#23885=CARTESIAN_POINT('Ctrl Pts',(120.670490053903,-125.383761285266,-83.8309820047469));
#23886=CARTESIAN_POINT('Ctrl Pts',(120.655933159391,-125.390886237448,-83.8423139630833));
#23887=CARTESIAN_POINT('Ctrl Pts',(120.641306624739,-125.398042702867,-83.8534937861162));
#23888=CARTESIAN_POINT('Ctrl Pts',(120.62662193437,-125.405224965794,-83.8645207217808));
#23889=CARTESIAN_POINT('Ctrl Pts',(120.623763587428,-125.406622979559,-83.8666670937534));
#23890=CARTESIAN_POINT('Ctrl Pts',(120.62090288229,-125.40802204969,-83.8688077929118));
#23891=CARTESIAN_POINT('Ctrl Pts',(120.618039908549,-125.409422131597,-83.8709428055742));
#23892=CARTESIAN_POINT('Ctrl Pts',(120.561761358575,-125.436944067424,-83.9129115512497));
#23893=CARTESIAN_POINT('Ctrl Pts',(120.504422162933,-125.464947521896,-83.9528770557978));
#23894=CARTESIAN_POINT('Ctrl Pts',(120.446193115433,-125.493345150898,-83.9910922510515));
#23895=CARTESIAN_POINT('Ctrl Pts',(120.399258153871,-125.516234785589,-84.0218952402353));
#23896=CARTESIAN_POINT('Ctrl Pts',(120.351744177111,-125.539380959607,-84.0515603444805));
#23897=CARTESIAN_POINT('Ctrl Pts',(120.303722804547,-125.562746846771,-84.0802057525297));
#23898=CARTESIAN_POINT('Ctrl Pts',(120.237604852662,-125.594918034739,-84.1196460186027));
#23899=CARTESIAN_POINT('Ctrl Pts',(120.170523556422,-125.627506495568,-84.157152051961));
#23900=CARTESIAN_POINT('Ctrl Pts',(120.102573990086,-125.660461610429,-84.1929593090859));
#23901=CARTESIAN_POINT('Ctrl Pts',(120.054961757024,-125.683553245799,-84.2180494393614));
#23902=CARTESIAN_POINT('Ctrl Pts',(120.006922336468,-125.706825340362,-84.24230479924));
#23903=CARTESIAN_POINT('Ctrl Pts',(119.958477373249,-125.73026591296,-84.2657976274669));
#23904=CARTESIAN_POINT('Ctrl Pts',(119.957432170273,-125.730771644714,-84.2663044866393));
#23905=CARTESIAN_POINT('Ctrl Pts',(119.956386759699,-125.731277463805,-84.2668109935507));
#23906=CARTESIAN_POINT('Ctrl Pts',(119.955341143413,-125.731783369317,-84.2673171481935));
#23907=CARTESIAN_POINT('Ctrl Pts',(119.89298150186,-125.761955131908,-84.2975037687741));
#23908=CARTESIAN_POINT('Ctrl Pts',(119.829839678401,-125.792457959603,-84.3264634103549));
#23909=CARTESIAN_POINT('Ctrl Pts',(119.766290102992,-125.823110100769,-84.3541852883539));
#23910=CARTESIAN_POINT('Ctrl Pts',(119.706671564982,-125.85186616769,-84.3801923517616));
#23911=CARTESIAN_POINT('Ctrl Pts',(119.646693089753,-125.880754168446,-84.4051101569439));
#23912=CARTESIAN_POINT('Ctrl Pts',(119.586626434295,-125.909641987124,-84.4289275235297));
#23913=CARTESIAN_POINT('Ctrl Pts',(119.501128626528,-125.950760393823,-84.4628287390101));
#23914=CARTESIAN_POINT('Ctrl Pts',(119.415197450966,-125.99200199476,-84.4946555586855));
#23915=CARTESIAN_POINT('Ctrl Pts',(119.328730569191,-126.033415379519,-84.5246645405908));
#23916=CARTESIAN_POINT('Ctrl Pts',(119.297298692445,-126.048469702963,-84.5355732099122));
#23917=CARTESIAN_POINT('Ctrl Pts',(119.265795758865,-126.063546844264,-84.5462412487785));
#23918=CARTESIAN_POINT('Ctrl Pts',(119.2342159707,-126.078649522118,-84.5566796096831));
#23919=CARTESIAN_POINT('Ctrl Pts',(119.1303530696,-126.12832078426,-84.5910103797511));
#23920=CARTESIAN_POINT('Ctrl Pts',(119.025943929888,-126.178130418089,-84.6227652061912));
#23921=CARTESIAN_POINT('Ctrl Pts',(118.920995425667,-126.22807113596,-84.6522643594006));
#23922=CARTESIAN_POINT('Ctrl Pts',(118.879152593278,-126.247982435342,-84.6640256334897));
#23923=CARTESIAN_POINT('Ctrl Pts',(118.8372237143,-126.267914711427,-84.6754278512292));
#23924=CARTESIAN_POINT('Ctrl Pts',(118.795208048995,-126.287868028778,-84.686489443114));
#23925=CARTESIAN_POINT('Ctrl Pts',(118.687953257482,-126.338803528117,-84.7147267380079));
#23926=CARTESIAN_POINT('Ctrl Pts',(118.579924099557,-126.389974247259,-84.7407679174261));
#23927=CARTESIAN_POINT('Ctrl Pts',(118.471295931363,-126.441294374164,-84.7647575879222));
#23928=CARTESIAN_POINT('Ctrl Pts',(118.355734714612,-126.495889940006,-84.7902783672747));
#23929=CARTESIAN_POINT('Ctrl Pts',(118.23949519911,-126.550654804836,-84.8134776148356));
#23930=CARTESIAN_POINT('Ctrl Pts',(118.122742883492,-126.605505675963,-84.8344961205875));
#23931=CARTESIAN_POINT('Ctrl Pts',(118.065228912499,-126.632526051483,-84.8448501570254));
#23932=CARTESIAN_POINT('Ctrl Pts',(118.007589863374,-126.659567573598,-84.854674480348));
#23933=CARTESIAN_POINT('Ctrl Pts',(117.949842319793,-126.686621640133,-84.8639830042662));
#23934=CARTESIAN_POINT('Ctrl Pts',(117.876606796367,-126.720931648848,-84.8757880885902));
#23935=CARTESIAN_POINT('Ctrl Pts',(117.803387560177,-126.755173054075,-84.8867590613586));
#23936=CARTESIAN_POINT('Ctrl Pts',(117.730135337143,-126.789368961517,-84.896927988525));
#23937=CARTESIAN_POINT('Ctrl Pts',(117.430682221293,-126.929160910605,-84.9384982890397));
#23938=CARTESIAN_POINT('Ctrl Pts',(117.129946638445,-127.068588179086,-84.9667803784096));
#23939=CARTESIAN_POINT('Ctrl Pts',(116.828007611095,-127.20757466619,-84.9830546227486));
#23940=CARTESIAN_POINT('Ctrl Pts',(116.615757672273,-127.305276091686,-84.9944947051906));
#23941=CARTESIAN_POINT('Ctrl Pts',(116.402913050166,-127.402759565481,-85.));
#23942=CARTESIAN_POINT('Ctrl Pts',(116.189500386222,-127.5,-85.));
#23943=CARTESIAN_POINT('Origin',(177.5,-127.5,85.));
#23944=CARTESIAN_POINT('Origin',(177.5,-127.5,73.9644660940673));
#23945=CARTESIAN_POINT('Origin',(177.5,-125.,73.9644660940673));
#23946=CARTESIAN_POINT('Origin',(177.5,-127.5,73.9644660940673));
#23947=CARTESIAN_POINT('Origin',(173.232233047034,-137.5,78.2322330470336));
#23948=CARTESIAN_POINT('Origin',(168.964466094067,-137.5,82.5));
#23949=CARTESIAN_POINT('Origin',(0.,-137.5,-82.5));
#23950=CARTESIAN_POINT('Ctrl Pts',(104.163333279998,-137.5,-85.));
#23951=CARTESIAN_POINT('Ctrl Pts',(103.738099080441,-137.661068405961,-85.));
#23952=CARTESIAN_POINT('Ctrl Pts',(103.313784132472,-137.820236149174,-84.9848502161634));
#23953=CARTESIAN_POINT('Ctrl Pts',(102.890445132596,-137.977529707376,-84.9541805579568));
#23954=CARTESIAN_POINT('Ctrl Pts',(102.674532847161,-138.057752913,-84.9385383515953));
#23955=CARTESIAN_POINT('Ctrl Pts',(102.458874713662,-138.137488523029,-84.9188583125581));
#23956=CARTESIAN_POINT('Ctrl Pts',(102.243480097268,-138.216739650426,-84.8950864427477));
#23957=CARTESIAN_POINT('Ctrl Pts',(102.169808729557,-138.243845894054,-84.8869557559584));
#23958=CARTESIAN_POINT('Ctrl Pts',(102.096197177396,-138.270885582569,-84.8783493800412));
#23959=CARTESIAN_POINT('Ctrl Pts',(102.022632569934,-138.297863659494,-84.8692643545073));
#23960=CARTESIAN_POINT('Ctrl Pts',(101.824799549342,-138.370414232822,-84.8448325236913));
#23961=CARTESIAN_POINT('Ctrl Pts',(101.627311999894,-138.442516995573,-84.8168822159707));
#23962=CARTESIAN_POINT('Ctrl Pts',(101.42999704102,-138.514238577898,-84.7850438375703));
#23963=CARTESIAN_POINT('Ctrl Pts',(101.276966125295,-138.569863450352,-84.7603510508216));
#23964=CARTESIAN_POINT('Ctrl Pts',(101.124039180306,-138.625258921571,-84.7333188027895));
#23965=CARTESIAN_POINT('Ctrl Pts',(100.971140292634,-138.680453268945,-84.7037536341508));
#23966=CARTESIAN_POINT('Ctrl Pts',(100.819413206494,-138.735224612453,-84.6744150499591));
#23967=CARTESIAN_POINT('Ctrl Pts',(100.667483749192,-138.789877248555,-84.6424995110724));
#23968=CARTESIAN_POINT('Ctrl Pts',(100.516166836934,-138.844125833747,-84.6079054671296));
#23969=CARTESIAN_POINT('Ctrl Pts',(100.456828089701,-138.865399351931,-84.5943394539282));
#23970=CARTESIAN_POINT('Ctrl Pts',(100.397584005817,-138.886610562357,-84.5803613497262));
#23971=CARTESIAN_POINT('Ctrl Pts',(100.338485741259,-138.907741516914,-84.565964289852));
#23972=CARTESIAN_POINT('Ctrl Pts',(100.220918177777,-138.949778535426,-84.5373233938226));
#23973=CARTESIAN_POINT('Ctrl Pts',(100.103632370179,-138.991604254091,-84.5069540658058));
#23974=CARTESIAN_POINT('Ctrl Pts',(99.9869935660692,-139.033088789031,-84.4747498712919));
#23975=CARTESIAN_POINT('Ctrl Pts',(99.9720326094956,-139.038409902621,-84.4706191228734));
#23976=CARTESIAN_POINT('Ctrl Pts',(99.9570823608136,-139.043725379489,-84.4664581642972));
#23977=CARTESIAN_POINT('Ctrl Pts',(99.9421436485644,-139.049034924161,-84.4622667514209));
#23978=CARTESIAN_POINT('Ctrl Pts',(99.8232112700053,-139.0913060896,-84.4288974291803));
#23979=CARTESIAN_POINT('Ctrl Pts',(99.7047475328351,-139.133296386698,-84.3935836754955));
#23980=CARTESIAN_POINT('Ctrl Pts',(99.5868591110941,-139.174972397689,-84.3559924242641));
#23981=CARTESIAN_POINT('Ctrl Pts',(99.5255437217676,-139.196648664126,-84.336440697551));
#23982=CARTESIAN_POINT('Ctrl Pts',(99.4643844621158,-139.218239730484,-84.3162722626081));
#23983=CARTESIAN_POINT('Ctrl Pts',(99.4033998553792,-139.239739634851,-84.2954359997591));
#23984=CARTESIAN_POINT('Ctrl Pts',(99.3132315996693,-139.271528129989,-84.2646287259707));
#23985=CARTESIAN_POINT('Ctrl Pts',(99.223535776852,-139.303085592255,-84.2323955368028));
#23986=CARTESIAN_POINT('Ctrl Pts',(99.1342049110009,-139.334451631701,-84.1984942631106));
#23987=CARTESIAN_POINT('Ctrl Pts',(99.0808040909447,-139.353201838725,-84.1782285263033));
#23988=CARTESIAN_POINT('Ctrl Pts',(99.0275342339471,-139.371883428182,-84.1573660209767));
#23989=CARTESIAN_POINT('Ctrl Pts',(98.9743778992268,-139.390502757733,-84.1358481968094));
#23990=CARTESIAN_POINT('Ctrl Pts',(98.8981671957289,-139.417197453882,-84.1049979034971));
#23991=CARTESIAN_POINT('Ctrl Pts',(98.8224769045325,-139.443662996202,-84.0729177573328));
#23992=CARTESIAN_POINT('Ctrl Pts',(98.7474387368693,-139.46985661819,-84.0394249607335));
#23993=CARTESIAN_POINT('Ctrl Pts',(98.6761330066818,-139.4947473558,-84.0075981132516));
#23994=CARTESIAN_POINT('Ctrl Pts',(98.6054159170073,-139.519392616372,-83.9744956741588));
#23995=CARTESIAN_POINT('Ctrl Pts',(98.5354408951835,-139.543741578814,-83.9399393538181));
#23996=CARTESIAN_POINT('Ctrl Pts',(98.5230520237326,-139.548052490877,-83.9338212591129));
#23997=CARTESIAN_POINT('Ctrl Pts',(98.5106865249416,-139.552354076384,-83.9276575341684));
#23998=CARTESIAN_POINT('Ctrl Pts',(98.4983453996891,-139.556646001529,-83.921447113738));
#23999=CARTESIAN_POINT('Ctrl Pts',(98.4332103940779,-139.579298276965,-83.8886692461367));
#24000=CARTESIAN_POINT('Ctrl Pts',(98.3686986921717,-139.601700795348,-83.8545667766362));
#24001=CARTESIAN_POINT('Ctrl Pts',(98.3049498142096,-139.623806785601,-83.8189431096019));
#24002=CARTESIAN_POINT('Ctrl Pts',(98.2461451146523,-139.644198299252,-83.7860823110428));
#24003=CARTESIAN_POINT('Ctrl Pts',(98.1879895705334,-139.664337465922,-83.7519270259336));
#24004=CARTESIAN_POINT('Ctrl Pts',(98.1306351301536,-139.684172991867,-83.7163018099732));
#24005=CARTESIAN_POINT('Ctrl Pts',(98.1258128865628,-139.685840722163,-83.7133065149586));
#24006=CARTESIAN_POINT('Ctrl Pts',(98.1209963324925,-139.687506296946,-83.710300816007));
#24007=CARTESIAN_POINT('Ctrl Pts',(98.1161855731307,-139.689169680641,-83.7072846016472));
#24008=CARTESIAN_POINT('Ctrl Pts',(98.1011329199801,-139.694374334612,-83.697847000393));
#24009=CARTESIAN_POINT('Ctrl Pts',(98.0861233722941,-139.699562258723,-83.6882946516978));
#24010=CARTESIAN_POINT('Ctrl Pts',(98.0711656112444,-139.704730507617,-83.6786258523484));
#24011=CARTESIAN_POINT('Ctrl Pts',(98.0285985107537,-139.719438415389,-83.6511101865903));
#24012=CARTESIAN_POINT('Ctrl Pts',(97.9864063827793,-139.734002420143,-83.6226254451987));
#24013=CARTESIAN_POINT('Ctrl Pts',(97.9447745948348,-139.748359981237,-83.5930927466016));
#24014=CARTESIAN_POINT('Ctrl Pts',(97.9055854441768,-139.761875149636,-83.5652928025733));
#24015=CARTESIAN_POINT('Ctrl Pts',(97.8668926229667,-139.775207447803,-83.5365641602674));
#24016=CARTESIAN_POINT('Ctrl Pts',(97.828893412403,-139.788290019043,-83.5068350472078));
#24017=CARTESIAN_POINT('Ctrl Pts',(97.804144005828,-139.796810876973,-83.4874720684692));
#24018=CARTESIAN_POINT('Ctrl Pts',(97.7796896932354,-139.805225503118,-83.4676845636184));
#24019=CARTESIAN_POINT('Ctrl Pts',(97.7555963200441,-139.813511537342,-83.4474515115311));
#24020=CARTESIAN_POINT('Ctrl Pts',(97.728363634325,-139.822877223255,-83.424582138104));
#24021=CARTESIAN_POINT('Ctrl Pts',(97.7016349752933,-139.832064017308,-83.4011923028985));
#24022=CARTESIAN_POINT('Ctrl Pts',(97.6754851218662,-139.841046916235,-83.3772268830841));
#24023=CARTESIAN_POINT('Ctrl Pts',(97.6463215006398,-139.851065093299,-83.3504994512098));
#24024=CARTESIAN_POINT('Ctrl Pts',(97.6179056267942,-139.860816746996,-83.3230936650656));
#24025=CARTESIAN_POINT('Ctrl Pts',(97.5902935806194,-139.87028550355,-83.2948558990642));
#24026=CARTESIAN_POINT('Ctrl Pts',(97.5639466259767,-139.879320433372,-83.2679118929831));
#24027=CARTESIAN_POINT('Ctrl Pts',(97.5383314014496,-139.88809782761,-83.2402104364255));
#24028=CARTESIAN_POINT('Ctrl Pts',(97.5135388526037,-139.896588714057,-83.2116040346635));
#24029=CARTESIAN_POINT('Ctrl Pts',(97.4980774724969,-139.901883886554,-83.1937642210211));
#24030=CARTESIAN_POINT('Ctrl Pts',(97.4829368794924,-139.907067340337,-83.17557218315));
#24031=CARTESIAN_POINT('Ctrl Pts',(97.4681484941753,-139.91212881033,-83.1569890466364));
#24032=CARTESIAN_POINT('Ctrl Pts',(97.4476130510072,-139.919157267269,-83.1311841372042));
#24033=CARTESIAN_POINT('Ctrl Pts',(97.4277452420287,-139.925954449789,-83.1045520895884));
#24034=CARTESIAN_POINT('Ctrl Pts',(97.4087167048375,-139.932462814289,-83.0770775195449));
#24035=CARTESIAN_POINT('Ctrl Pts',(97.3896881676464,-139.938971178789,-83.0496029495014));
#24036=CARTESIAN_POINT('Ctrl Pts',(97.3714983087636,-139.945190921619,-83.0212855162084));
#24037=CARTESIAN_POINT('Ctrl Pts',(97.3543677310461,-139.951047779757,-82.9921212813803));
#24038=CARTESIAN_POINT('Ctrl Pts',(97.3386981110691,-139.956405143811,-82.9654442781753));
#24039=CARTESIAN_POINT('Ctrl Pts',(97.3240367075897,-139.961419891151,-82.9382531572));
#24040=CARTESIAN_POINT('Ctrl Pts',(97.3105164866214,-139.966044132201,-82.910533567852));
#24041=CARTESIAN_POINT('Ctrl Pts',(97.2987364265489,-139.970073196333,-82.8863817120154));
#24042=CARTESIAN_POINT('Ctrl Pts',(97.2878230738592,-139.973805693467,-82.8618285577111));
#24043=CARTESIAN_POINT('Ctrl Pts',(97.277894901901,-139.977199920877,-82.8368687469214));
#24044=CARTESIAN_POINT('Ctrl Pts',(97.2675449135807,-139.980738358185,-82.8108484733772));
#24045=CARTESIAN_POINT('Ctrl Pts',(97.2582088704294,-139.983928680802,-82.7843403311583));
#24046=CARTESIAN_POINT('Ctrl Pts',(97.2499984542927,-139.986731261435,-82.757268617013));
#24047=CARTESIAN_POINT('Ctrl Pts',(97.2412356636815,-139.989722392072,-82.7283755915447));
#24048=CARTESIAN_POINT('Ctrl Pts',(97.2338238173965,-139.992251733102,-82.6990112555058));
#24049=CARTESIAN_POINT('Ctrl Pts',(97.2279126563665,-139.99426861304,-82.6692964230559));
#24050=CARTESIAN_POINT('Ctrl Pts',(97.2221710252593,-139.996227649603,-82.6404338010639));
#24051=CARTESIAN_POINT('Ctrl Pts',(97.2178453353219,-139.997703166035,-82.6112405024812));
#24052=CARTESIAN_POINT('Ctrl Pts',(97.2150271728466,-139.998664330779,-82.5818324954324));
#24053=CARTESIAN_POINT('Ctrl Pts',(97.21242764044,-139.999550929378,-82.5547059305124));
#24054=CARTESIAN_POINT('Ctrl Pts',(97.2111104751974,-140.,-82.5273967255209));
#24055=CARTESIAN_POINT('Ctrl Pts',(97.2111104761178,-140.,-82.5));
#24056=CARTESIAN_POINT('Origin',(0.,0.,-87.5));
#24057=CARTESIAN_POINT('Origin',(104.163333279998,-137.5,-87.5));
#24058=CARTESIAN_POINT('Origin',(116.189500386223,-127.5,-87.5));
#24059=CARTESIAN_POINT('Ctrl Pts',(119.689439203101,-120.724637681159,-82.5));
#24060=CARTESIAN_POINT('Ctrl Pts',(115.377099114166,-125.,-82.5));
#24061=CARTESIAN_POINT('Ctrl Pts',(121.449578014911,-125.,-82.5));
#24062=CARTESIAN_POINT('Ctrl Pts',(119.689439200917,-120.724637683324,-82.7056798133782));
#24063=CARTESIAN_POINT('Ctrl Pts',(115.377099118341,-124.999999995701,-82.3507082521197));
#24064=CARTESIAN_POINT('Ctrl Pts',(121.449578012695,-125.,-82.6028399066646));
#24065=CARTESIAN_POINT('Ctrl Pts',(119.676882557983,-120.737090180421,-82.9079954286207));
#24066=CARTESIAN_POINT('Ctrl Pts',(115.401361881511,-124.975048941511,-82.2053610116202));
#24067=CARTESIAN_POINT('Ctrl Pts',(121.436836713265,-125.006317811859,-82.7039977143433));
#24068=CARTESIAN_POINT('Ctrl Pts',(119.628410587298,-120.785117230515,-83.3063417968652));
#24069=CARTESIAN_POINT('Ctrl Pts',(115.489012547634,-124.884856124345,-81.9514922386294));
#24070=CARTESIAN_POINT('Ctrl Pts',(121.387651919446,-125.030684477513,-82.9031708983997));
#24071=CARTESIAN_POINT('Ctrl Pts',(119.592485604525,-120.820701126369,-83.5023756354685));
#24072=CARTESIAN_POINT('Ctrl Pts',(115.551419916513,-124.820623886438,-81.844093442978));
#24073=CARTESIAN_POINT('Ctrl Pts',(121.351198628156,-125.048738071447,-83.0011878177447));
#24074=CARTESIAN_POINT('Ctrl Pts',(119.497801818693,-120.91434900059,-83.8883271564993));
#24075=CARTESIAN_POINT('Ctrl Pts',(115.697825563992,-124.669744960185,-81.6876871655071));
#24076=CARTESIAN_POINT('Ctrl Pts',(121.255122433638,-125.096250595907,-83.1941635782393));
#24077=CARTESIAN_POINT('Ctrl Pts',(119.439376348876,-120.972080469663,-84.0761788301475));
#24078=CARTESIAN_POINT('Ctrl Pts',(115.779889571829,-124.585091209873,-81.639444465222));
#24079=CARTESIAN_POINT('Ctrl Pts',(121.195837765812,-125.125540825988,-83.2880894152805));
#24080=CARTESIAN_POINT('Ctrl Pts',(119.305221428487,-121.104388919918,-84.4342801401529));
#24081=CARTESIAN_POINT('Ctrl Pts',(115.940258775456,-124.419250986645,-81.6056236890861));
#24082=CARTESIAN_POINT('Ctrl Pts',(121.059709978865,-125.192667908432,-83.4671400698696));
#24083=CARTESIAN_POINT('Ctrl Pts',(119.229146767872,-121.179307379907,-84.6059387232763));
#24084=CARTESIAN_POINT('Ctrl Pts',(116.018662098376,-124.337976550129,-81.6177805257506));
#24085=CARTESIAN_POINT('Ctrl Pts',(120.982516573327,-125.230678008636,-83.5529693617978));
#24086=CARTESIAN_POINT('Ctrl Pts',(119.060491893051,-121.345017393603,-84.9357796688685));
#24087=CARTESIAN_POINT('Ctrl Pts',(116.159254888288,-124.191486350903,-81.6927658265867));
#24088=CARTESIAN_POINT('Ctrl Pts',(120.811381479668,-125.314751472042,-83.7178898342746));
#24089=CARTESIAN_POINT('Ctrl Pts',(118.96776206845,-121.435951457507,-85.093861858456));
#24090=CARTESIAN_POINT('Ctrl Pts',(116.221496701314,-124.12623198531,-81.7541916577615));
#24091=CARTESIAN_POINT('Ctrl Pts',(120.717287981259,-125.36088713601,-83.7969309295804));
#24092=CARTESIAN_POINT('Ctrl Pts',(118.772148188168,-121.627281202587,-85.3899146057789));
#24093=CARTESIAN_POINT('Ctrl Pts',(116.320002770212,-124.021697634043,-81.9095222659674));
#24094=CARTESIAN_POINT('Ctrl Pts',(120.518797426192,-125.45795884595,-83.9449573025371));
#24095=CARTESIAN_POINT('Ctrl Pts',(118.66868983755,-121.728242289117,-85.5290754975167));
#24096=CARTESIAN_POINT('Ctrl Pts',(116.35752640374,-123.981145420879,-82.0023320413466));
#24097=CARTESIAN_POINT('Ctrl Pts',(120.413817629313,-125.50918174931,-84.0145377490307));
#24098=CARTESIAN_POINT('Ctrl Pts',(118.45169839953,-121.939403249423,-85.7917547211079));
#24099=CARTESIAN_POINT('Ctrl Pts',(116.406873166747,-123.925571355125,-82.2074570860312));
#24100=CARTESIAN_POINT('Ctrl Pts',(120.193635140666,-125.616314884214,-84.1458773602816));
#24101=CARTESIAN_POINT('Ctrl Pts',(118.338158476483,-122.049610026221,-85.9152619328964));
#24102=CARTESIAN_POINT('Ctrl Pts',(116.419520677459,-123.909734352817,-82.3190059601612));
#24103=CARTESIAN_POINT('Ctrl Pts',(120.078425512936,-125.672228616066,-84.2076309666417));
#24104=CARTESIAN_POINT('Ctrl Pts',(118.101739972007,-122.278395780866,-86.1479296435188));
#24105=CARTESIAN_POINT('Ctrl Pts',(116.420156575106,-123.902371131663,-82.5520650696801));
#24106=CARTESIAN_POINT('Ctrl Pts',(119.838530265679,-125.788303741941,-84.323964821566));
#24107=CARTESIAN_POINT('Ctrl Pts',(117.978621353548,-122.397201959151,-86.2571677342239));
#24108=CARTESIAN_POINT('Ctrl Pts',(116.408784821067,-123.910208556756,-82.6734238697007));
#24109=CARTESIAN_POINT('Ctrl Pts',(119.713601079353,-125.848580405477,-84.3785838674499));
#24110=CARTESIAN_POINT('Ctrl Pts',(117.603241895162,-122.758291253176,-86.5592543593046));
#24111=CARTESIAN_POINT('Ctrl Pts',(116.343210235511,-123.964762276173,-83.0296153459409));
#24112=CARTESIAN_POINT('Ctrl Pts',(119.332701334762,-126.031780121634,-84.5296271789764));
#24113=CARTESIAN_POINT('Ctrl Pts',(117.342767505456,-123.007368772318,-86.7291564746629));
#24114=CARTESIAN_POINT('Ctrl Pts',(116.259553389397,-124.040181684855,-83.2697315003776));
#24115=CARTESIAN_POINT('Ctrl Pts',(119.068396439392,-126.158150332831,-84.6145782376957));
#24116=CARTESIAN_POINT('Ctrl Pts',(116.804336290701,-123.518763278367,-87.016825817368));
#24117=CARTESIAN_POINT('Ctrl Pts',(116.02736829311,-124.252946369571,-83.719666170302));
#24118=CARTESIAN_POINT('Ctrl Pts',(118.522047118472,-126.417607839943,-84.7584129083197));
#24119=CARTESIAN_POINT('Ctrl Pts',(116.525023660541,-123.782353191699,-87.1348755768559));
#24120=CARTESIAN_POINT('Ctrl Pts',(115.881406957192,-124.387808755614,-83.9325453429328));
#24121=CARTESIAN_POINT('Ctrl Pts',(118.238626949673,-126.551340957402,-84.8174377888648));
#24122=CARTESIAN_POINT('Ctrl Pts',(115.671272356593,-124.582362934983,-87.4141780079963));
#24123=CARTESIAN_POINT('Ctrl Pts',(115.387279747815,-124.844116246409,-84.4905439734664));
#24124=CARTESIAN_POINT('Ctrl Pts',(117.372320479471,-126.95722825408,-84.9570890031244));
#24125=CARTESIAN_POINT('Ctrl Pts',(115.092722580527,-125.117129923752,-87.4999999999441));
#24126=CARTESIAN_POINT('Ctrl Pts',(114.975356365159,-125.224084605229,-84.7914664637583));
#24127=CARTESIAN_POINT('Ctrl Pts',(116.785263550907,-127.228543433487,-85.));
#24128=CARTESIAN_POINT('Ctrl Pts',(114.505594583524,-125.652173913043,-87.5));
#24129=CARTESIAN_POINT('Ctrl Pts',(114.505594583524,-125.652173913043,-85.));
#24130=CARTESIAN_POINT('Ctrl Pts',(116.189500386222,-127.5,-85.));
#24131=CARTESIAN_POINT('Origin',(177.5,-127.5,73.9644660940673));
#24132=CARTESIAN_POINT('Origin',(177.5,-127.5,73.9644660940673));
#24133=CARTESIAN_POINT('Origin',(168.964466094067,-137.5,82.5));
#24134=CARTESIAN_POINT('Origin',(168.964466094067,-137.5,82.5));
#24135=CARTESIAN_POINT('Origin',(168.964466094067,-137.5,82.5));
#24136=CARTESIAN_POINT('Ctrl Pts',(102.653719754201,-135.507246376812,-87.5));
#24137=CARTESIAN_POINT('Ctrl Pts',(102.653719754201,-135.507246376812,-85.));
#24138=CARTESIAN_POINT('Ctrl Pts',(104.163333279998,-137.5,-85.));
#24139=CARTESIAN_POINT('Ctrl Pts',(101.942824967883,-136.045785799024,-87.4999999986499));
#24140=CARTESIAN_POINT('Ctrl Pts',(102.098115024429,-135.928145581712,-85.2088536164867));
#24141=CARTESIAN_POINT('Ctrl Pts',(103.441984205064,-137.773229542126,-85.));
#24142=CARTESIAN_POINT('Ctrl Pts',(101.239352594638,-136.569897864386,-87.412786288228));
#24143=CARTESIAN_POINT('Ctrl Pts',(101.486609565828,-136.386099347641,-85.331905314613));
#24144=CARTESIAN_POINT('Ctrl Pts',(102.728166603362,-138.039139357556,-84.9563931437868));
#24145=CARTESIAN_POINT('Ctrl Pts',(100.196407749732,-137.334867215748,-87.1513844296707));
#24146=CARTESIAN_POINT('Ctrl Pts',(100.54257036391,-137.08212804413,-85.3647787687136));
#24147=CARTESIAN_POINT('Ctrl Pts',(101.669884334297,-138.427248808045,-84.825692214999));
#24148=CARTESIAN_POINT('Ctrl Pts',(99.8508244887539,-137.58630689324,-87.0421034532917));
#24149=CARTESIAN_POINT('Ctrl Pts',(100.230398916982,-137.310719986095,-85.3526237075885));
#24150=CARTESIAN_POINT('Ctrl Pts',(101.319218966522,-138.554817467693,-84.7710517262891));
#24151=CARTESIAN_POINT('Ctrl Pts',(99.1647702284533,-138.081596677989,-86.7728948774191));
#24152=CARTESIAN_POINT('Ctrl Pts',(99.6048287382421,-137.765412086316,-85.2762415031115));
#24153=CARTESIAN_POINT('Ctrl Pts',(100.623075672997,-138.806104197121,-84.6364474390664));
#24154=CARTESIAN_POINT('Ctrl Pts',(98.8231223087188,-138.326258685221,-86.6120988871654));
#24155=CARTESIAN_POINT('Ctrl Pts',(99.2895441365193,-137.992946799803,-85.2128933853019));
#24156=CARTESIAN_POINT('Ctrl Pts',(100.276403519106,-138.930234185559,-84.5560494432021));
#24157=CARTESIAN_POINT('Ctrl Pts',(98.1642932033775,-138.794578008566,-86.236965419431));
#24158=CARTESIAN_POINT('Ctrl Pts',(98.6779850295722,-138.431144249613,-85.0309421888964));
#24159=CARTESIAN_POINT('Ctrl Pts',(99.6078857505209,-139.167837372319,-84.3684827100962));
#24160=CARTESIAN_POINT('Ctrl Pts',(97.8450871550092,-139.019702589725,-86.0223563343333));
#24161=CARTESIAN_POINT('Ctrl Pts',(98.3787305056279,-138.644046161722,-84.9137267915435));
#24162=CARTESIAN_POINT('Ctrl Pts',(99.283985495488,-139.28205498953,-84.2611781664592));
#24163=CARTESIAN_POINT('Ctrl Pts',(97.2348460956408,-139.447206832062,-85.5210364529044));
#24164=CARTESIAN_POINT('Ctrl Pts',(97.8048933229574,-139.049632684085,-84.6126732163398));
#24165=CARTESIAN_POINT('Ctrl Pts',(98.6647703029657,-139.498950525936,-84.0105182271597));
#24166=CARTESIAN_POINT('Ctrl Pts',(96.9485250987458,-139.646264128654,-85.2381599055602));
#24167=CARTESIAN_POINT('Ctrl Pts',(97.5330426499524,-139.240425205481,-84.4318673801205));
#24168=CARTESIAN_POINT('Ctrl Pts',(98.3742387030706,-139.599942828535,-83.869079952008));
#24169=CARTESIAN_POINT('Ctrl Pts',(96.5670588723941,-139.910067692477,-84.7527693623909));
#24170=CARTESIAN_POINT('Ctrl Pts',(97.1694267365962,-139.49429609941,-84.1046276840804));
#24171=CARTESIAN_POINT('Ctrl Pts',(97.9871626793753,-139.7337843447,-83.6263846815815));
#24172=CARTESIAN_POINT('Ctrl Pts',(96.446921948779,-139.992887137954,-84.5790592166605));
#24173=CARTESIAN_POINT('Ctrl Pts',(97.0550355767484,-139.573924747954,-83.985796851679));
#24174=CARTESIAN_POINT('Ctrl Pts',(97.8652590362145,-139.775803032622,-83.5395296080959));
#24175=CARTESIAN_POINT('Ctrl Pts',(96.230792082191,-140.141542227306,-84.2107293038302));
#24176=CARTESIAN_POINT('Ctrl Pts',(96.8492338219199,-139.716869275045,-83.7297846724926));
#24177=CARTESIAN_POINT('Ctrl Pts',(97.6459507893286,-139.851223630635,-83.3553646521495));
#24178=CARTESIAN_POINT('Ctrl Pts',(96.1354852319174,-140.20691083986,-84.0176816842604));
#24179=CARTESIAN_POINT('Ctrl Pts',(96.7581590378938,-139.779958879001,-83.5936364082725));
#24180=CARTESIAN_POINT('Ctrl Pts',(97.5492423676424,-139.884388586841,-83.2588408418563));
#24181=CARTESIAN_POINT('Ctrl Pts',(95.9757708369295,-140.316288364145,-83.6101822300658));
#24182=CARTESIAN_POINT('Ctrl Pts',(96.6056940387067,-139.885419084152,-83.3034331025056));
#24183=CARTESIAN_POINT('Ctrl Pts',(97.3871792316287,-139.939881597544,-83.0550911153068));
#24184=CARTESIAN_POINT('Ctrl Pts',(95.9112233305706,-140.360393155342,-83.3934903679299));
#24185=CARTESIAN_POINT('Ctrl Pts',(96.5438567051695,-139.928100230385,-83.1474982708776));
#24186=CARTESIAN_POINT('Ctrl Pts',(97.3216824971681,-139.962258291636,-82.9467451839126));
#24187=CARTESIAN_POINT('Ctrl Pts',(95.8249655550993,-140.419296052404,-82.9539654903595));
#24188=CARTESIAN_POINT('Ctrl Pts',(96.4613838167463,-139.984990149168,-82.8298756349127));
#24189=CARTESIAN_POINT('Ctrl Pts',(97.2341562250557,-139.99214285053,-82.7269827452321));
#24190=CARTESIAN_POINT('Ctrl Pts',(95.802253798755,-140.434782611285,-82.7294636530625));
#24191=CARTESIAN_POINT('Ctrl Pts',(96.4395937226627,-140.0000000025,-82.6666388430675));
#24192=CARTESIAN_POINT('Ctrl Pts',(97.2111104722631,-140.,-82.6147318264911));
#24193=CARTESIAN_POINT('Ctrl Pts',(95.802253802551,-140.434782608696,-82.5));
#24194=CARTESIAN_POINT('Ctrl Pts',(96.4395937263074,-140.,-82.5));
#24195=CARTESIAN_POINT('Ctrl Pts',(97.2111104761179,-140.,-82.5));
#24196=CARTESIAN_POINT('Origin',(97.2111104761179,-142.5,-82.5));
#24197=CARTESIAN_POINT('Origin',(140.840826156048,-127.5,110.623639938019));
#24198=CARTESIAN_POINT('Origin',(168.964466094067,-127.5,82.5));
#24199=CARTESIAN_POINT('Origin',(168.964466094067,0.,82.5));
#24200=CARTESIAN_POINT('Origin',(168.964466094067,-127.5,82.5));
#24201=CARTESIAN_POINT('Origin',(180.,-137.5,82.5));
#24202=CARTESIAN_POINT('Ctrl Pts',(97.2111104761179,-140.,82.5));
#24203=CARTESIAN_POINT('Ctrl Pts',(97.2111104761179,-140.,82.6755496768536));
#24204=CARTESIAN_POINT('Ctrl Pts',(97.2669993053863,-139.980948398877,82.8433669193193));
#24205=CARTESIAN_POINT('Ctrl Pts',(97.4416750152787,-139.921239210978,83.1407858319269));
#24206=CARTESIAN_POINT('Ctrl Pts',(97.5528693408584,-139.883166869044,83.2647663586162));
#24207=CARTESIAN_POINT('Ctrl Pts',(97.7975572341499,-139.799120034918,83.4891405228876));
#24208=CARTESIAN_POINT('Ctrl Pts',(97.9325262666959,-139.752638285023,83.5889920461804));
#24209=CARTESIAN_POINT('Ctrl Pts',(98.2091898573102,-139.657040028271,83.7678569462812));
#24210=CARTESIAN_POINT('Ctrl Pts',(98.3521285688953,-139.607498613007,83.8477491623104));
#24211=CARTESIAN_POINT('Ctrl Pts',(98.7901601853575,-139.455163852716,84.0681986935237));
#24212=CARTESIAN_POINT('Ctrl Pts',(99.0953089605357,-139.348355708036,84.1900813067333));
#24213=CARTESIAN_POINT('Ctrl Pts',(99.7103269532128,-139.131535702876,84.4002328533732));
#24214=CARTESIAN_POINT('Ctrl Pts',(100.021642419245,-139.021028910904,84.4887015138217));
#24215=CARTESIAN_POINT('Ctrl Pts',(100.963515042103,-138.68428076857,84.7184070178217));
#24216=CARTESIAN_POINT('Ctrl Pts',(101.60311676071,-138.452377890846,84.8244784333066));
#24217=CARTESIAN_POINT('Ctrl Pts',(102.880937057798,-137.982203598024,84.9652998446299));
#24218=CARTESIAN_POINT('Ctrl Pts',(103.521414707761,-137.743143193377,85.));
#24219=CARTESIAN_POINT('Ctrl Pts',(104.163333279998,-137.5,85.));
#24220=CARTESIAN_POINT('Origin',(97.2111104761179,-142.5,115.));
#24221=CARTESIAN_POINT('Origin',(97.2111104761179,-142.5,82.5));
#24222=CARTESIAN_POINT('Origin',(121.449578014911,-122.5,-49.5));
#24223=CARTESIAN_POINT('Origin',(121.449578014911,-122.5,-49.5));
#24224=CARTESIAN_POINT('Origin',(121.449578014911,-122.5,-49.5));
#24225=CARTESIAN_POINT('Origin',(168.964466094067,-127.5,82.5));
#24226=CARTESIAN_POINT('Origin',(168.964466094067,-127.5,82.5));
#24227=CARTESIAN_POINT('Ctrl Pts',(95.8063843937655,-140.431966711357,82.3302220946682));
#24228=CARTESIAN_POINT('Ctrl Pts',(96.4436693342528,-139.997193891514,82.3767164474287));
#24229=CARTESIAN_POINT('Ctrl Pts',(97.2155465823485,-139.998571769581,82.4151232270192));
#24230=CARTESIAN_POINT('Ctrl Pts',(95.7923535903208,-140.44153068871,82.6189757789366));
#24231=CARTESIAN_POINT('Ctrl Pts',(96.4301984592196,-140.006470158917,82.5862803340826));
#24232=CARTESIAN_POINT('Ctrl Pts',(97.2013093103815,-140.003422681504,82.5594793863882));
#24233=CARTESIAN_POINT('Ctrl Pts',(95.8143433314503,-140.426549686738,82.8999538047621));
#24234=CARTESIAN_POINT('Ctrl Pts',(96.451370555694,-139.991898168234,82.7909496905922));
#24235=CARTESIAN_POINT('Ctrl Pts',(97.2236226187951,-139.995824235922,82.69994805132));
#24236=CARTESIAN_POINT('Ctrl Pts',(95.9113524568369,-140.360304954438,83.3940569629634));
#24237=CARTESIAN_POINT('Ctrl Pts',(96.5440906351144,-139.927939556875,83.1478648493756));
#24238=CARTESIAN_POINT('Ctrl Pts',(97.3220593832045,-139.962224365005,82.9469649889257));
#24239=CARTESIAN_POINT('Ctrl Pts',(95.9760732771133,-140.316081550096,83.6111084029453));
#24240=CARTESIAN_POINT('Ctrl Pts',(96.6060933643896,-139.88514399948,83.3040436736954));
#24241=CARTESIAN_POINT('Ctrl Pts',(97.3877326179702,-139.939793891199,83.0554758102092));
#24242=CARTESIAN_POINT('Ctrl Pts',(96.1359171968624,-140.206614708383,84.0186285797908));
#24243=CARTESIAN_POINT('Ctrl Pts',(96.7586808353661,-139.779598324237,83.5942322269066));
#24244=CARTESIAN_POINT('Ctrl Pts',(97.549928900367,-139.884271165605,83.2592091881112));
#24245=CARTESIAN_POINT('Ctrl Pts',(96.2312574439685,-140.141222656174,84.2116073129497));
#24246=CARTESIAN_POINT('Ctrl Pts',(96.8497861981093,-139.716486932324,83.7303149679427));
#24247=CARTESIAN_POINT('Ctrl Pts',(97.6466721866358,-139.851103576304,83.3556865024526));
#24248=CARTESIAN_POINT('Ctrl Pts',(96.4473504048935,-139.992591935039,84.5797041056106));
#24249=CARTESIAN_POINT('Ctrl Pts',(97.0555509298913,-139.573566933705,83.9861341719472));
#24250=CARTESIAN_POINT('Ctrl Pts',(97.8659453704935,-139.775715999607,83.5397134594335));
#24251=CARTESIAN_POINT('Ctrl Pts',(96.5679243919307,-139.909470610042,84.7539893762804));
#24252=CARTESIAN_POINT('Ctrl Pts',(97.170358683852,-139.493647616232,84.1053449301989));
#24253=CARTESIAN_POINT('Ctrl Pts',(97.9882938037511,-139.733555567922,83.6268467456624));
#24254=CARTESIAN_POINT('Ctrl Pts',(96.9500803569823,-139.645185630464,85.2398999355275));
#24255=CARTESIAN_POINT('Ctrl Pts',(97.5346293969998,-139.239315047688,84.4328697043282));
#24256=CARTESIAN_POINT('Ctrl Pts',(98.3760735528311,-139.599505523373,83.8697781593213));
#24257=CARTESIAN_POINT('Ctrl Pts',(97.2354525040957,-139.44678671983,85.5216876072768));
#24258=CARTESIAN_POINT('Ctrl Pts',(97.8055901602141,-139.049145300856,84.6129417193528));
#24259=CARTESIAN_POINT('Ctrl Pts',(98.6656453772965,-139.498873185454,84.0106618938605));
#24260=CARTESIAN_POINT('Ctrl Pts',(97.84736130348,-139.018104706215,86.0240708677892));
#24261=CARTESIAN_POINT('Ctrl Pts',(98.3809815624723,-138.642451119717,84.9145219274169));
#24262=CARTESIAN_POINT('Ctrl Pts',(99.2865604725242,-139.281432946434,84.2618427002277));
#24263=CARTESIAN_POINT('Ctrl Pts',(98.166043362077,-138.793333891558,86.2379611602865));
#24264=CARTESIAN_POINT('Ctrl Pts',(98.6796642081939,-138.429941914644,85.0311843476465));
#24265=CARTESIAN_POINT('Ctrl Pts',(99.6099329912234,-139.167421255509,84.3687873468945));
#24266=CARTESIAN_POINT('Ctrl Pts',(98.8213488187872,-138.327519386904,86.6110898616138));
#24267=CARTESIAN_POINT('Ctrl Pts',(99.2879449246068,-137.99409288667,85.2121201908167));
#24268=CARTESIAN_POINT('Ctrl Pts',(100.27488438625,-138.931140045816,84.5553582822027));
#24269=CARTESIAN_POINT('Ctrl Pts',(99.1580967027271,-138.086393592505,86.7699896797119));
#24270=CARTESIAN_POINT('Ctrl Pts',(99.598826751245,-137.769758011627,85.2749349361932));
#24271=CARTESIAN_POINT('Ctrl Pts',(100.616589177685,-138.808829045632,84.6348154491461));
#24272=CARTESIAN_POINT('Ctrl Pts',(99.8465457819706,-137.589416498873,87.0407064600204));
#24273=CARTESIAN_POINT('Ctrl Pts',(100.226641408901,-137.313468734571,85.3520865086701));
#24274=CARTESIAN_POINT('Ctrl Pts',(101.3151733035,-138.556733152654,84.7701949757436));
#24275=CARTESIAN_POINT('Ctrl Pts',(100.196958385717,-137.33447257932,87.1516264431956));
#24276=CARTESIAN_POINT('Ctrl Pts',(100.543205603977,-137.081667395925,85.3644982653917));
#24277=CARTESIAN_POINT('Ctrl Pts',(101.670744758202,-138.427408643403,84.8256690051307));
#24278=CARTESIAN_POINT('Ctrl Pts',(101.288218386673,-136.534036534848,87.4248120559258));
#24279=CARTESIAN_POINT('Ctrl Pts',(101.533114418443,-136.351795325559,85.3295920701954));
#24280=CARTESIAN_POINT('Ctrl Pts',(102.778066848937,-138.021368555809,84.9623127946856));
#24281=CARTESIAN_POINT('Ctrl Pts',(102.034252820327,-135.97755865104,87.5102062320107));
#24282=CARTESIAN_POINT('Ctrl Pts',(102.179857181174,-135.866853574868,85.1905835680137));
#24283=CARTESIAN_POINT('Ctrl Pts',(103.535087152153,-137.739070348775,85.0050578474458));
#24284=CARTESIAN_POINT('Ctrl Pts',(102.78362116352,-135.408741267552,87.4990307673126));
#24285=CARTESIAN_POINT('Ctrl Pts',(102.759250409394,-135.427238236656,84.9584361067191));
#24286=CARTESIAN_POINT('Ctrl Pts',(104.295502567804,-137.450494181459,84.9995248789653));
#24287=CARTESIAN_POINT('Origin',(104.163333279998,-137.5,87.5));
#24288=CARTESIAN_POINT('Origin',(0.,0.,-49.5));
#24289=CARTESIAN_POINT('Origin',(147.5,-89.4427190999916,-49.5));
#24290=CARTESIAN_POINT('Origin',(147.5,0.,-44.5));
#24291=CARTESIAN_POINT('Origin',(147.5,-122.5,-44.5));
#24292=CARTESIAN_POINT('Ctrl Pts',(150.,-80.6225774829854,-44.5));
#24293=CARTESIAN_POINT('Ctrl Pts',(150.,-80.6225774829854,-44.5312343888304));
#24294=CARTESIAN_POINT('Ctrl Pts',(149.999418286665,-80.6247797743348,-44.5621210164789));
#24295=CARTESIAN_POINT('Ctrl Pts',(149.998293554945,-80.6290354954265,-44.5925723355625));
#24296=CARTESIAN_POINT('Ctrl Pts',(149.997125538082,-80.6334549973542,-44.6241955694378));
#24297=CARTESIAN_POINT('Ctrl Pts',(149.995371936956,-80.6400888791781,-44.655349356458));
#24298=CARTESIAN_POINT('Ctrl Pts',(149.993090530187,-80.6487160556979,-44.6859412124329));
#24299=CARTESIAN_POINT('Ctrl Pts',(149.992231155702,-80.6519657941861,-44.6974647429366));
#24300=CARTESIAN_POINT('Ctrl Pts',(149.991297028852,-80.6554978429527,-44.7089085934095));
#24301=CARTESIAN_POINT('Ctrl Pts',(149.990291719683,-80.6592985775913,-44.7202680068894));
#24302=CARTESIAN_POINT('Ctrl Pts',(149.987499102739,-80.6698565196466,-44.7518229668389));
#24303=CARTESIAN_POINT('Ctrl Pts',(149.984157100677,-80.6824881297728,-44.7827141728588));
#24304=CARTESIAN_POINT('Ctrl Pts',(149.980355786964,-80.6968505802923,-44.8128256266941));
#24305=CARTESIAN_POINT('Ctrl Pts',(149.977558137322,-80.7074209008703,-44.8349867279405));
#24306=CARTESIAN_POINT('Ctrl Pts',(149.974509955706,-80.7189351701335,-44.8567449506927));
#24307=CARTESIAN_POINT('Ctrl Pts',(149.971243495187,-80.7312708109915,-44.8780946805967));
#24308=CARTESIAN_POINT('Ctrl Pts',(149.965898079908,-80.7514575307578,-44.9130325504344));
#24309=CARTESIAN_POINT('Ctrl Pts',(149.960009186179,-80.773686648641,-44.9465704967713));
#24310=CARTESIAN_POINT('Ctrl Pts',(149.953740444404,-80.797335293561,-44.9787015735967));
#24311=CARTESIAN_POINT('Ctrl Pts',(149.948225014278,-80.8181420923231,-45.0069714745479));
#24312=CARTESIAN_POINT('Ctrl Pts',(149.9424154207,-80.8400482470994,-45.0341525202745));
#24313=CARTESIAN_POINT('Ctrl Pts',(149.936415096464,-80.8626613647233,-45.0602466352771));
#24314=CARTESIAN_POINT('Ctrl Pts',(149.930229230798,-80.8859737229195,-45.0871476299065));
#24315=CARTESIAN_POINT('Ctrl Pts',(149.923781601043,-80.9102578633712,-45.1131530185116));
#24316=CARTESIAN_POINT('Ctrl Pts',(149.917129634266,-80.9352949903539,-45.1383421170535));
#24317=CARTESIAN_POINT('Ctrl Pts',(149.910169623638,-80.9614915538295,-45.1646976896917));
#24318=CARTESIAN_POINT('Ctrl Pts',(149.902985851619,-80.9885126935503,-45.1901596664586));
#24319=CARTESIAN_POINT('Ctrl Pts',(149.895629953764,-81.0161619977713,-45.2148125956205));
#24320=CARTESIAN_POINT('Ctrl Pts',(149.894768894784,-81.0193985410376,-45.2176983923565));
#24321=CARTESIAN_POINT('Ctrl Pts',(149.893905462669,-81.0226437475977,-45.2205730959881));
#24322=CARTESIAN_POINT('Ctrl Pts',(149.893039728921,-81.0258973457795,-45.2234368363464));
#24323=CARTESIAN_POINT('Ctrl Pts',(149.885294621979,-81.055004985282,-45.2490566939069));
#24324=CARTESIAN_POINT('Ctrl Pts',(149.877335285324,-81.0848961910411,-45.2738874208924));
#24325=CARTESIAN_POINT('Ctrl Pts',(149.869211724912,-81.1153826082176,-45.2979942587922));
#24326=CARTESIAN_POINT('Ctrl Pts',(149.860756318493,-81.1471143901477,-45.3230858567598));
#24327=CARTESIAN_POINT('Ctrl Pts',(149.852122887,-81.179491428094,-45.3473933229362));
#24328=CARTESIAN_POINT('Ctrl Pts',(149.843353240441,-81.212356779593,-45.3709861423032));
#24329=CARTESIAN_POINT('Ctrl Pts',(149.834033859779,-81.2472823286657,-45.3960579012523));
#24330=CARTESIAN_POINT('Ctrl Pts',(149.824560562659,-81.282759673792,-45.420322766943));
#24331=CARTESIAN_POINT('Ctrl Pts',(149.814968902639,-81.318656015993,-45.4438574826091));
#24332=CARTESIAN_POINT('Ctrl Pts',(149.814245534136,-81.3213631890219,-45.4456323862228));
#24333=CARTESIAN_POINT('Ctrl Pts',(149.813521486337,-81.3240727682655,-45.4474031333746));
#24334=CARTESIAN_POINT('Ctrl Pts',(149.81279677161,-81.3267847076918,-45.4491697551619));
#24335=CARTESIAN_POINT('Ctrl Pts',(149.802161746897,-81.3665818053887,-45.4750945303171));
#24336=CARTESIAN_POINT('Ctrl Pts',(149.791378236576,-81.4068954418303,-45.5001449499175));
#24337=CARTESIAN_POINT('Ctrl Pts',(149.780505488345,-81.4474999785173,-45.5243508763432));
#24338=CARTESIAN_POINT('Ctrl Pts',(149.766212096436,-81.5008789903218,-45.5561721588362));
#24339=CARTESIAN_POINT('Ctrl Pts',(149.75173104415,-81.5548874755347,-45.5866585651915));
#24340=CARTESIAN_POINT('Ctrl Pts',(149.7370901728,-81.6094178533078,-45.6160154789332));
#24341=CARTESIAN_POINT('Ctrl Pts',(149.721679195218,-81.6668165155371,-45.6469165591158));
#24342=CARTESIAN_POINT('Ctrl Pts',(149.706091100881,-81.7247936014321,-45.6765660851853));
#24343=CARTESIAN_POINT('Ctrl Pts',(149.690345642873,-81.7832715016962,-45.7051731327433));
#24344=CARTESIAN_POINT('Ctrl Pts',(149.684002656688,-81.8068290579963,-45.7166973518138));
#24345=CARTESIAN_POINT('Ctrl Pts',(149.67763399788,-81.8304683944407,-45.7280520707485));
#24346=CARTESIAN_POINT('Ctrl Pts',(149.671240444102,-81.854186356593,-45.7392497349255));
#24347=CARTESIAN_POINT('Ctrl Pts',(149.663115656512,-81.8843266214971,-45.7534794803999));
#24348=CARTESIAN_POINT('Ctrl Pts',(149.654955183208,-81.9145791058626,-45.7674477491405));
#24349=CARTESIAN_POINT('Ctrl Pts',(149.646761444289,-81.9449339838539,-45.7811773107384));
#24350=CARTESIAN_POINT('Ctrl Pts',(149.629599044989,-82.0085145472401,-45.8099349048783));
#24351=CARTESIAN_POINT('Ctrl Pts',(149.612256027528,-82.0726719053374,-45.8376821506386));
#24352=CARTESIAN_POINT('Ctrl Pts',(149.594776281623,-82.1372383448953,-45.8645156723128));
#24353=CARTESIAN_POINT('Ctrl Pts',(149.57592605508,-82.2068670465535,-45.8934530473311));
#24354=CARTESIAN_POINT('Ctrl Pts',(149.556916727547,-82.2769718987423,-45.9213279816653));
#24355=CARTESIAN_POINT('Ctrl Pts',(149.537787182918,-82.3473991049663,-45.9482460618992));
#24356=CARTESIAN_POINT('Ctrl Pts',(149.532245072383,-82.3678029028159,-45.9560446257929));
#24357=CARTESIAN_POINT('Ctrl Pts',(149.526692780135,-82.3882340721267,-45.9637627732937));
#24358=CARTESIAN_POINT('Ctrl Pts',(149.521131044556,-82.4086895813368,-45.9714028195526));
#24359=CARTESIAN_POINT('Ctrl Pts',(149.513307047732,-82.4374654619684,-45.9821504893812));
#24360=CARTESIAN_POINT('Ctrl Pts',(149.505462657808,-82.4662967316413,-45.9927459306726));
#24361=CARTESIAN_POINT('Ctrl Pts',(149.497602582526,-82.4951656239004,-46.0031912460791));
#24362=CARTESIAN_POINT('Ctrl Pts',(149.466886299739,-82.6079819808148,-46.0440103540796));
#24363=CARTESIAN_POINT('Ctrl Pts',(149.435949796432,-82.721306238521,-46.0825462658463));
#24364=CARTESIAN_POINT('Ctrl Pts',(149.404819096531,-82.8350358342389,-46.1191658716245));
#24365=CARTESIAN_POINT('Ctrl Pts',(149.382928718768,-82.9150078175565,-46.1449159192168));
#24366=CARTESIAN_POINT('Ctrl Pts',(149.360942099001,-82.995181007926,-46.169717455523));
#24367=CARTESIAN_POINT('Ctrl Pts',(149.338865605393,-83.0755291035976,-46.193686300737));
#24368=CARTESIAN_POINT('Ctrl Pts',(149.30257270251,-83.2076182697843,-46.233090156576));
#24369=CARTESIAN_POINT('Ctrl Pts',(149.266041574139,-83.3401623692395,-46.2702654172594));
#24370=CARTESIAN_POINT('Ctrl Pts',(149.229255373738,-83.4732146574125,-46.3055170512346));
#24371=CARTESIAN_POINT('Ctrl Pts',(149.222100057115,-83.4990947765572,-46.3123738779743));
#24372=CARTESIAN_POINT('Ctrl Pts',(149.214935059986,-83.5249942184406,-46.3191578024711));
#24373=CARTESIAN_POINT('Ctrl Pts',(149.207760216038,-83.5509135089673,-46.3258708967128));
#24374=CARTESIAN_POINT('Ctrl Pts',(149.164019348336,-83.7089284102155,-46.366796743915));
#24375=CARTESIAN_POINT('Ctrl Pts',(149.119950314816,-83.8675446159544,-46.4050588777709));
#24376=CARTESIAN_POINT('Ctrl Pts',(149.075578120339,-84.0266555943282,-46.4410493230434));
#24377=CARTESIAN_POINT('Ctrl Pts',(149.050851325548,-84.1153215834145,-46.4611053145304));
#24378=CARTESIAN_POINT('Ctrl Pts',(149.026030206988,-84.2041418314762,-46.4804550867179));
#24379=CARTESIAN_POINT('Ctrl Pts',(149.001117827171,-84.2931021083258,-46.4991611413161));
#24380=CARTESIAN_POINT('Ctrl Pts',(148.961812515426,-84.4334584869728,-46.5286744721549));
#24381=CARTESIAN_POINT('Ctrl Pts',(148.922228706232,-84.5743409203763,-46.5565824640166));
#24382=CARTESIAN_POINT('Ctrl Pts',(148.882458149795,-84.7154243069172,-46.58297626425));
#24383=CARTESIAN_POINT('Ctrl Pts',(148.823378480021,-84.9250054803839,-46.6221845917561));
#24384=CARTESIAN_POINT('Ctrl Pts',(148.763691428381,-85.1357176965639,-46.658180607518));
#24385=CARTESIAN_POINT('Ctrl Pts',(148.703725142332,-85.346373256235,-46.6911268937745));
#24386=CARTESIAN_POINT('Ctrl Pts',(148.683093735236,-85.4188493239555,-46.7024620670668));
#24387=CARTESIAN_POINT('Ctrl Pts',(148.662429146923,-85.4913191022908,-46.7134360383522));
#24388=CARTESIAN_POINT('Ctrl Pts',(148.64174438629,-85.5637353575988,-46.7240548006858));
#24389=CARTESIAN_POINT('Ctrl Pts',(148.565624143843,-85.8302283090543,-46.7631320120529));
#24390=CARTESIAN_POINT('Ctrl Pts',(148.489028565031,-86.0967324995911,-46.7975654258511));
#24391=CARTESIAN_POINT('Ctrl Pts',(148.411875341988,-86.3635238183437,-46.8277812265461));
#24392=CARTESIAN_POINT('Ctrl Pts',(148.365096720961,-86.5252815453832,-46.846101310063));
#24393=CARTESIAN_POINT('Ctrl Pts',(148.318112978006,-86.6871449972432,-46.8628698580675));
#24394=CARTESIAN_POINT('Ctrl Pts',(148.270904619886,-86.8491769961467,-46.8781728422293));
#24395=CARTESIAN_POINT('Ctrl Pts',(148.24918654488,-86.9237193705385,-46.8852129379044));
#24396=CARTESIAN_POINT('Ctrl Pts',(148.227421070419,-86.9982969676292,-46.8919477958447));
#24397=CARTESIAN_POINT('Ctrl Pts',(148.205605817643,-87.0729174681581,-46.8983780579096));
#24398=CARTESIAN_POINT('Ctrl Pts',(148.10190068443,-87.42764766667,-46.9289461742125));
#24399=CARTESIAN_POINT('Ctrl Pts',(147.997167488693,-87.7829762387816,-46.9525973445083));
#24400=CARTESIAN_POINT('Ctrl Pts',(147.891499227195,-88.1385323929249,-46.969351029831));
#24401=CARTESIAN_POINT('Ctrl Pts',(147.785745335364,-88.4943766789206,-46.9861182918287));
#24402=CARTESIAN_POINT('Ctrl Pts',(147.679054863979,-88.8504488649393,-46.9959768816863));
#24403=CARTESIAN_POINT('Ctrl Pts',(147.571529965735,-89.2063722196095,-46.9989975290796));
#24404=CARTESIAN_POINT('Ctrl Pts',(147.547727111398,-89.285163196442,-46.9996662116924));
#24405=CARTESIAN_POINT('Ctrl Pts',(147.523883400528,-89.3639468619846,-47.));
#24406=CARTESIAN_POINT('Ctrl Pts',(147.5,-89.4427190999916,-47.));
#24407=CARTESIAN_POINT('Origin',(115.217186218029,-122.5,-49.5));
#24408=CARTESIAN_POINT('Origin',(147.5,-122.5,-49.5));
#24409=CARTESIAN_POINT('Origin',(115.217186218029,-127.5,82.5));
#24410=CARTESIAN_POINT('Ctrl Pts',(116.189500386223,-127.5,85.));
#24411=CARTESIAN_POINT('Ctrl Pts',(116.448008540164,-127.382212026451,85.));
#24412=CARTESIAN_POINT('Ctrl Pts',(116.70545859626,-127.26417086413,84.9919054816509));
#24413=CARTESIAN_POINT('Ctrl Pts',(116.961798715612,-127.145925914751,84.9750282599701));
#24414=CARTESIAN_POINT('Ctrl Pts',(117.203993376622,-127.034206003318,84.9590823635802));
#24415=CARTESIAN_POINT('Ctrl Pts',(117.44519709308,-126.922304463616,84.9352961059057));
#24416=CARTESIAN_POINT('Ctrl Pts',(117.685352827265,-126.810270254864,84.9030396161985));
#24417=CARTESIAN_POINT('Ctrl Pts',(117.699379201419,-126.803726860281,84.9011556653736));
#24418=CARTESIAN_POINT('Ctrl Pts',(117.713401997064,-126.797183014578,84.8992428067277));
#24419=CARTESIAN_POINT('Ctrl Pts',(117.727421201483,-126.790638727994,84.897300909382));
#24420=CARTESIAN_POINT('Ctrl Pts',(117.801716706967,-126.755956939695,84.8870097230499));
#24421=CARTESIAN_POINT('Ctrl Pts',(117.875811770813,-126.721306222531,84.8759163529931));
#24422=CARTESIAN_POINT('Ctrl Pts',(117.949766484243,-126.686659174451,84.8639959183815));
#24423=CARTESIAN_POINT('Ctrl Pts',(118.06803595945,-126.631251100998,84.8449325824511));
#24424=CARTESIAN_POINT('Ctrl Pts',(118.186129688142,-126.575765453057,84.8236742085113));
#24425=CARTESIAN_POINT('Ctrl Pts',(118.304009972734,-126.520223268699,84.8000156545051));
#24426=CARTESIAN_POINT('Ctrl Pts',(118.414673338094,-126.468081512665,84.7778055350189));
#24427=CARTESIAN_POINT('Ctrl Pts',(118.525149041361,-126.41588969173,84.7534800370994));
#24428=CARTESIAN_POINT('Ctrl Pts',(118.635381578924,-126.363674712089,84.7268318520061));
#24429=CARTESIAN_POINT('Ctrl Pts',(118.688420413194,-126.338551262036,84.714009969248));
#24430=CARTESIAN_POINT('Ctrl Pts',(118.741402540217,-126.313422617291,84.7006497952873));
#24431=CARTESIAN_POINT('Ctrl Pts',(118.794319125548,-126.288292874885,84.6867249125825));
#24432=CARTESIAN_POINT('Ctrl Pts',(118.899018286902,-126.238571923722,84.6591735592211));
#24433=CARTESIAN_POINT('Ctrl Pts',(119.002876811871,-126.189124992078,84.6295858023581));
#24434=CARTESIAN_POINT('Ctrl Pts',(119.105920148838,-126.139946013067,84.5977086876102));
#24435=CARTESIAN_POINT('Ctrl Pts',(119.148229575818,-126.119753204074,84.5846199960125));
#24436=CARTESIAN_POINT('Ctrl Pts',(119.190401214644,-126.099605728966,84.5711448947681));
#24437=CARTESIAN_POINT('Ctrl Pts',(119.232435280194,-126.079503870074,84.5572639252337));
#24438=CARTESIAN_POINT('Ctrl Pts',(119.332253758341,-126.031767898399,84.5243007265521));
#24439=CARTESIAN_POINT('Ctrl Pts',(119.431308801167,-125.984284516995,84.4890488616751));
#24440=CARTESIAN_POINT('Ctrl Pts',(119.529560384222,-125.937075343632,84.4512249355722));
#24441=CARTESIAN_POINT('Ctrl Pts',(119.549179492571,-125.927648504302,84.4436721646005));
#24442=CARTESIAN_POINT('Ctrl Pts',(119.56876646678,-125.918232645463,84.4360167122299));
#24443=CARTESIAN_POINT('Ctrl Pts',(119.588320838716,-125.908828011419,84.4282561299977));
#24444=CARTESIAN_POINT('Ctrl Pts',(119.676176605169,-125.866573965376,84.3933886383497));
#24445=CARTESIAN_POINT('Ctrl Pts',(119.763367640996,-125.82454975495,84.3563903280491));
#24446=CARTESIAN_POINT('Ctrl Pts',(119.849778269297,-125.782813941846,84.3169432875038));
#24447=CARTESIAN_POINT('Ctrl Pts',(119.88415418401,-125.766210582052,84.3012504482301));
#24448=CARTESIAN_POINT('Ctrl Pts',(119.918406261816,-125.749653027032,84.2851696439165));
#24449=CARTESIAN_POINT('Ctrl Pts',(119.952525858354,-125.73314564101,84.2686790921243));
#24450=CARTESIAN_POINT('Ctrl Pts',(119.95435634409,-125.732260034563,84.2677943888189));
#24451=CARTESIAN_POINT('Ctrl Pts',(119.956186462171,-125.731374563089,84.2669084964009));
#24452=CARTESIAN_POINT('Ctrl Pts',(119.958016213969,-125.730489226021,84.2660214100548));
#24453=CARTESIAN_POINT('Ctrl Pts',(120.016911873286,-125.701992185948,84.2374680645808));
#24454=CARTESIAN_POINT('Ctrl Pts',(120.075514267379,-125.673592123274,84.2076160589798));
#24455=CARTESIAN_POINT('Ctrl Pts',(120.133520234546,-125.645440552611,84.1764738678677));
#24456=CARTESIAN_POINT('Ctrl Pts',(120.185326529706,-125.620297819024,84.1486601510473));
#24457=CARTESIAN_POINT('Ctrl Pts',(120.236657062466,-125.595353295122,84.1198170381164));
#24458=CARTESIAN_POINT('Ctrl Pts',(120.287252932459,-125.570735521273,84.0899486390561));
#24459=CARTESIAN_POINT('Ctrl Pts',(120.29330775259,-125.567789506258,84.0863742804385));
#24460=CARTESIAN_POINT('Ctrl Pts',(120.299351995964,-125.564848197438,84.0827852387161));
#24461=CARTESIAN_POINT('Ctrl Pts',(120.305385171907,-125.561911837745,84.0791815213283));
#24462=CARTESIAN_POINT('Ctrl Pts',(120.36056980737,-125.535053357114,84.046218811097));
#24463=CARTESIAN_POINT('Ctrl Pts',(120.414989618081,-125.508531012063,84.0119891408571));
#24464=CARTESIAN_POINT('Ctrl Pts',(120.468555276,-125.482393019785,83.9762964268862));
#24465=CARTESIAN_POINT('Ctrl Pts',(120.521845432222,-125.456389461797,83.9407872895508));
#24466=CARTESIAN_POINT('Ctrl Pts',(120.574290544872,-125.430766130924,83.9038303719441));
#24467=CARTESIAN_POINT('Ctrl Pts',(120.625763505242,-125.405589684656,83.8652058122217));
#24468=CARTESIAN_POINT('Ctrl Pts',(120.669724343261,-125.38408756649,83.8322182396925));
#24469=CARTESIAN_POINT('Ctrl Pts',(120.712919977829,-125.362939699079,83.798058607416));
#24470=CARTESIAN_POINT('Ctrl Pts',(120.755308589242,-125.342167431342,83.7625256624148));
#24471=CARTESIAN_POINT('Ctrl Pts',(120.796119057626,-125.322168522496,83.7283156215514));
#24472=CARTESIAN_POINT('Ctrl Pts',(120.836181594618,-125.302517695486,83.6928327066558));
#24473=CARTESIAN_POINT('Ctrl Pts',(120.87542145341,-125.283252598435,83.6558720771839));
#24474=CARTESIAN_POINT('Ctrl Pts',(120.882694505626,-125.279681839999,83.649021476893));
#24475=CARTESIAN_POINT('Ctrl Pts',(120.889939185317,-125.276124387987,83.6421200366677));
#24476=CARTESIAN_POINT('Ctrl Pts',(120.897154862446,-125.27258055919,83.6351663481078));
#24477=CARTESIAN_POINT('Ctrl Pts',(120.930420737947,-125.256242720701,83.603108298149));
#24478=CARTESIAN_POINT('Ctrl Pts',(120.962969894054,-125.240243618606,83.5699873690875));
#24479=CARTESIAN_POINT('Ctrl Pts',(120.994602600081,-125.224682872253,83.5357995420131));
#24480=CARTESIAN_POINT('Ctrl Pts',(121.024642658856,-125.209905580212,83.5033330077298));
#24481=CARTESIAN_POINT('Ctrl Pts',(121.053856347428,-125.195523551178,83.4699041218694));
#24482=CARTESIAN_POINT('Ctrl Pts',(121.082031519346,-125.181642679555,83.4355171688528));
#24483=CARTESIAN_POINT('Ctrl Pts',(121.097985602281,-125.173782689287,83.416045688717));
#24484=CARTESIAN_POINT('Ctrl Pts',(121.113605937311,-125.166083770035,83.3962671745771));
#24485=CARTESIAN_POINT('Ctrl Pts',(121.1288474274,-125.158568448299,83.3761839355069));
#24486=CARTESIAN_POINT('Ctrl Pts',(121.149706220237,-125.148283329307,83.3486989507179));
#24487=CARTESIAN_POINT('Ctrl Pts',(121.169911626188,-125.138314491271,83.3205937206656));
#24488=CARTESIAN_POINT('Ctrl Pts',(121.189383694812,-125.128702127376,83.2918112814197));
#24489=CARTESIAN_POINT('Ctrl Pts',(121.219288926705,-125.113939444639,83.2476071685062));
#24490=CARTESIAN_POINT('Ctrl Pts',(121.247502565816,-125.100002690991,83.201750806387));
#24491=CARTESIAN_POINT('Ctrl Pts',(121.273533474621,-125.08713705486,83.154295706818));
#24492=CARTESIAN_POINT('Ctrl Pts',(121.283706281684,-125.082109199894,83.1357503853428));
#24493=CARTESIAN_POINT('Ctrl Pts',(121.293546196337,-125.07724471837,83.1169610515117));
#24494=CARTESIAN_POINT('Ctrl Pts',(121.303025858184,-125.072557339689,83.0979315436973));
#24495=CARTESIAN_POINT('Ctrl Pts',(121.323095906417,-125.062633365845,83.0576428555715));
#24496=CARTESIAN_POINT('Ctrl Pts',(121.341528989802,-125.053514201567,83.0161861527192));
#24497=CARTESIAN_POINT('Ctrl Pts',(121.357996565716,-125.045363893225,82.9739496378786));
#24498=CARTESIAN_POINT('Ctrl Pts',(121.365145493259,-125.041825669743,82.9556138618141));
#24499=CARTESIAN_POINT('Ctrl Pts',(121.371924242049,-125.038469923387,82.9371317587732));
#24500=CARTESIAN_POINT('Ctrl Pts',(121.378307256224,-125.035309443556,82.9185377169621));
#24501=CARTESIAN_POINT('Ctrl Pts',(121.391447468896,-125.028803210607,82.8802596155576));
#24502=CARTESIAN_POINT('Ctrl Pts',(121.402999576331,-125.02308111907,82.8412451545452));
#24503=CARTESIAN_POINT('Ctrl Pts',(121.41267276749,-125.018288884737,82.8018442319798));
#24504=CARTESIAN_POINT('Ctrl Pts',(121.422709757883,-125.013316419171,82.7609614793595));
#24505=CARTESIAN_POINT('Ctrl Pts',(121.430817047113,-125.009299023442,82.7195176678589));
#24506=CARTESIAN_POINT('Ctrl Pts',(121.43683910078,-125.006314500199,82.6776303050308));
#24507=CARTESIAN_POINT('Ctrl Pts',(121.442766130939,-125.003377070502,82.6364038934916));
#24508=CARTESIAN_POINT('Ctrl Pts',(121.446673152333,-125.001440207745,82.5947478151296));
#24509=CARTESIAN_POINT('Ctrl Pts',(121.448457146603,-125.000555735143,82.5527767557765));
#24510=CARTESIAN_POINT('Ctrl Pts',(121.449202695032,-125.000186105503,82.5352366448472));
#24511=CARTESIAN_POINT('Ctrl Pts',(121.449578014743,-125.,82.5176415554239));
#24512=CARTESIAN_POINT('Ctrl Pts',(121.449578014911,-125.,82.5));
#24513=CARTESIAN_POINT('Origin',(0.,0.,87.5));
#24514=CARTESIAN_POINT('Origin',(116.189500386222,-127.5,87.5));
#24515=CARTESIAN_POINT('Ctrl Pts',(150.289855072464,-79.4541343310581,-44.5));
#24516=CARTESIAN_POINT('Ctrl Pts',(150.,-80.0024038100394,-44.5));
#24517=CARTESIAN_POINT('Ctrl Pts',(150.,-80.6225774829855,-44.5));
#24518=CARTESIAN_POINT('Ctrl Pts',(150.28985506853,-79.4541343384987,-44.7594238560556));
#24519=CARTESIAN_POINT('Ctrl Pts',(149.999999996126,-80.0024038172978,-44.6905851824362));
#24520=CARTESIAN_POINT('Ctrl Pts',(150.,-80.6225774905387,-44.629711927975));
#24521=CARTESIAN_POINT('Ctrl Pts',(150.270119749701,-79.4914922605508,-45.0111695802387));
#24522=CARTESIAN_POINT('Ctrl Pts',(149.980519833119,-80.0389466368966,-44.8758156770736));
#24523=CARTESIAN_POINT('Ctrl Pts',(149.989987226484,-80.6604847938369,-44.7555847901951));
#24524=CARTESIAN_POINT('Ctrl Pts',(150.196231486305,-79.6310132970258,-45.5012087006257));
#24525=CARTESIAN_POINT('Ctrl Pts',(149.907890955038,-80.1748646486434,-45.2336047942099));
#24526=CARTESIAN_POINT('Ctrl Pts',(149.952499797667,-80.8020576101747,-45.0006043502371));
#24527=CARTESIAN_POINT('Ctrl Pts',(150.143050717941,-79.7313168859281,-45.7320003431406));
#24528=CARTESIAN_POINT('Ctrl Pts',(149.855501091412,-80.272795283317,-45.4011397919881));
#24529=CARTESIAN_POINT('Ctrl Pts',(149.925518380098,-80.9038362519448,-45.1160001719023));
#24530=CARTESIAN_POINT('Ctrl Pts',(150.01502846971,-79.971931353987,-46.1617150079383));
#24531=CARTESIAN_POINT('Ctrl Pts',(149.729850869406,-80.506872138187,-45.7093793927994));
#24532=CARTESIAN_POINT('Ctrl Pts',(149.860565913637,-81.1479891679691,-45.3308575036371));
#24533=CARTESIAN_POINT('Ctrl Pts',(149.939105635844,-80.1142600764838,-46.3637363656926));
#24534=CARTESIAN_POINT('Ctrl Pts',(149.655266820466,-80.6454659182033,-45.8524984192499));
#24535=CARTESIAN_POINT('Ctrl Pts',(149.8220462428,-81.2924109599909,-45.4318681833206));
#24536=CARTESIAN_POINT('Ctrl Pts',(149.775363670977,-80.4199633406152,-46.7336380224264));
#24537=CARTESIAN_POINT('Ctrl Pts',(149.494928348598,-80.9422362487695,-46.1103934277676));
#24538=CARTESIAN_POINT('Ctrl Pts',(149.738971273161,-81.6026098603007,-45.616819010739));
#24539=CARTESIAN_POINT('Ctrl Pts',(149.686995608736,-80.5843780010491,-46.903585266663));
#24540=CARTESIAN_POINT('Ctrl Pts',(149.408398325687,-81.1018541496878,-46.2266925752405));
#24541=CARTESIAN_POINT('Ctrl Pts',(149.694137478568,-81.7694423834459,-45.7017926336777));
#24542=CARTESIAN_POINT('Ctrl Pts',(149.500255462679,-80.9302925286903,-47.2210941330543));
#24543=CARTESIAN_POINT('Ctrl Pts',(149.226078269656,-81.4367533718067,-46.4395269094013));
#24544=CARTESIAN_POINT('Ctrl Pts',(149.599394315017,-82.1204438893779,-45.8605470661809));
#24545=CARTESIAN_POINT('Ctrl Pts',(149.401347886678,-81.1127763961003,-47.369210707149));
#24546=CARTESIAN_POINT('Ctrl Pts',(149.129574349821,-81.6133256610688,-46.5363235480013));
#24547=CARTESIAN_POINT('Ctrl Pts',(149.549213266548,-82.3056113431187,-45.9346053539496));
#24548=CARTESIAN_POINT('Ctrl Pts',(149.197899201605,-81.4863922312653,-47.6435514113241));
#24549=CARTESIAN_POINT('Ctrl Pts',(148.93165319989,-81.9738530462045,-46.7107456147876));
#24550=CARTESIAN_POINT('Ctrl Pts',(149.445992976772,-82.684721528767,-46.071775705287));
#24551=CARTESIAN_POINT('Ctrl Pts',(149.093462145135,-81.6773447374821,-47.7698090460946));
#24552=CARTESIAN_POINT('Ctrl Pts',(148.830186520417,-82.1578926315274,-46.7883037911384));
#24553=CARTESIAN_POINT('Ctrl Pts',(149.393006529828,-82.8784821601051,-46.1349045233201));
#24554=CARTESIAN_POINT('Ctrl Pts',(148.773324875584,-82.2599185303359,-48.1224993059861));
#24555=CARTESIAN_POINT('Ctrl Pts',(148.518202139789,-82.721231742148,-46.9985052310704));
#24556=CARTESIAN_POINT('Ctrl Pts',(149.230583943609,-83.4696232145796,-46.3112496524474));
#24557=CARTESIAN_POINT('Ctrl Pts',(148.550873607932,-82.6611103319713,-48.3232112727545));
#24558=CARTESIAN_POINT('Ctrl Pts',(148.30315471628,-83.1060920248234,-47.1056075630378));
#24559=CARTESIAN_POINT('Ctrl Pts',(149.117722639557,-83.8767148956951,-46.4116056366651));
#24560=CARTESIAN_POINT('Ctrl Pts',(148.091214058598,-83.4818155626998,-48.6734332925097));
#24561=CARTESIAN_POINT('Ctrl Pts',(147.862495369544,-83.8874214153556,-47.2694844772005));
#24562=CARTESIAN_POINT('Ctrl Pts',(148.884513014786,-84.7094893209564,-46.586716645967));
#24563=CARTESIAN_POINT('Ctrl Pts',(147.853104568995,-83.9028862659541,-48.8228865658125));
#24564=CARTESIAN_POINT('Ctrl Pts',(147.635229789707,-84.286581928446,-47.3247069198698));
#24565=CARTESIAN_POINT('Ctrl Pts',(148.763707465283,-85.1367522404598,-46.6614432831528));
#24566=CARTESIAN_POINT('Ctrl Pts',(147.37234266623,-84.7444834282146,-49.073322172108));
#24567=CARTESIAN_POINT('Ctrl Pts',(147.180928816256,-85.0771956930355,-47.3874171310308));
#24568=CARTESIAN_POINT('Ctrl Pts',(148.519791499647,-85.9907258315643,-46.7866610858075));
#24569=CARTESIAN_POINT('Ctrl Pts',(147.128665473946,-85.166872640511,-49.1751382031672));
#24570=CARTESIAN_POINT('Ctrl Pts',(146.952267516978,-85.4713149459694,-47.3939268980417));
#24571=CARTESIAN_POINT('Ctrl Pts',(148.396161159612,-86.4193266499342,-46.837569101695));
#24572=CARTESIAN_POINT('Ctrl Pts',(146.388097896077,-86.4377602232181,-49.41873440213));
#24573=CARTESIAN_POINT('Ctrl Pts',(146.253862108763,-86.6644852388405,-47.3459550909554));
#24574=CARTESIAN_POINT('Ctrl Pts',(148.020432020732,-87.7089037559046,-46.9593672008422));
#24575=CARTESIAN_POINT('Ctrl Pts',(145.881711078451,-87.289917999924,-49.4999999990937));
#24576=CARTESIAN_POINT('Ctrl Pts',(145.791767290438,-87.4382443129923,-47.2157310733627));
#24577=CARTESIAN_POINT('Ctrl Pts',(147.763515165397,-88.573593311031,-47.));
#24578=CARTESIAN_POINT('Ctrl Pts',(145.36231884058,-88.1464478086874,-49.5));
#24579=CARTESIAN_POINT('Ctrl Pts',(145.36231884058,-88.1464478086874,-46.9999999999999));
#24580=CARTESIAN_POINT('Ctrl Pts',(147.5,-89.4427190999917,-47.));
#24581=CARTESIAN_POINT('Origin',(152.5,-80.6225774829854,-44.5));
#24582=CARTESIAN_POINT('Origin',(147.5,-122.5,-44.5));
#24583=CARTESIAN_POINT('Origin',(152.5,-122.5,-44.5));
#24584=CARTESIAN_POINT('Ctrl Pts',(114.505594583524,-125.652173913043,87.5));
#24585=CARTESIAN_POINT('Ctrl Pts',(114.505594583524,-125.652173913043,85.));
#24586=CARTESIAN_POINT('Ctrl Pts',(116.189500386223,-127.5,85.));
#24587=CARTESIAN_POINT('Ctrl Pts',(115.098666513066,-125.111713276286,87.4999999993277));
#24588=CARTESIAN_POINT('Ctrl Pts',(114.980468455817,-125.219426007098,84.789197137563));
#24589=CARTESIAN_POINT('Ctrl Pts',(116.791295074219,-127.225795199451,85.));
#24590=CARTESIAN_POINT('Ctrl Pts',(115.677248330338,-124.576762485165,87.412213589489));
#24591=CARTESIAN_POINT('Ctrl Pts',(115.390477170759,-124.841163526176,84.4869181320052));
#24592=CARTESIAN_POINT('Ctrl Pts',(117.378384335167,-126.95438684931,84.9561067940497));
#24593=CARTESIAN_POINT('Ctrl Pts',(116.521921487207,-123.785260415245,87.135895140949));
#24594=CARTESIAN_POINT('Ctrl Pts',(115.879476439134,-124.389591527255,83.9347335464724));
#24595=CARTESIAN_POINT('Ctrl Pts',(118.235479156151,-126.55281594586,84.8179475708219));
#24596=CARTESIAN_POINT('Ctrl Pts',(116.800657852356,-123.522253316268,87.0187226097786));
#24597=CARTESIAN_POINT('Ctrl Pts',(116.025791458688,-124.254393807365,83.7225655755012));
#24598=CARTESIAN_POINT('Ctrl Pts',(118.51831458544,-126.419378520877,84.7593613046283));
#24599=CARTESIAN_POINT('Ctrl Pts',(117.344689694216,-123.005546784036,86.728197778466));
#24600=CARTESIAN_POINT('Ctrl Pts',(116.260513692635,-124.039299071365,83.2680355386732));
#24601=CARTESIAN_POINT('Ctrl Pts',(119.07034689564,-126.157225941778,84.614098889494));
#24602=CARTESIAN_POINT('Ctrl Pts',(117.605972114118,-122.755671483612,86.5572347078813));
#24603=CARTESIAN_POINT('Ctrl Pts',(116.343854196171,-123.964200078231,83.0270891162914));
#24604=CARTESIAN_POINT('Ctrl Pts',(119.335471703983,-126.03045097373,84.5286173533875));
#24605=CARTESIAN_POINT('Ctrl Pts',(117.979759695143,-122.396103662867,86.2561620132639));
#24606=CARTESIAN_POINT('Ctrl Pts',(116.408893575195,-123.910132089279,82.6723188019316));
#24607=CARTESIAN_POINT('Ctrl Pts',(119.714756161272,-125.848023181682,84.3780810069086));
#24608=CARTESIAN_POINT('Ctrl Pts',(118.101314578112,-122.278806587615,86.1483179654515));
#24609=CARTESIAN_POINT('Ctrl Pts',(116.420127652017,-123.902387828605,82.5524859464439));
#24610=CARTESIAN_POINT('Ctrl Pts',(119.838098616002,-125.788512166127,84.3241589823631));
#24611=CARTESIAN_POINT('Ctrl Pts',(118.337674566632,-122.050079163152,85.9157683721022));
#24612=CARTESIAN_POINT('Ctrl Pts',(116.419552940987,-123.909688381786,82.3194835992922));
#24613=CARTESIAN_POINT('Ctrl Pts',(120.077934486753,-125.672466633894,84.2078841864137));
#24614=CARTESIAN_POINT('Ctrl Pts',(118.452813811185,-121.938320691333,85.7905474845089));
#24615=CARTESIAN_POINT('Ctrl Pts',(116.406751222331,-123.925725220725,82.2063383456538));
#24616=CARTESIAN_POINT('Ctrl Pts',(120.194766955428,-125.615765645109,84.1452737420412));
#24617=CARTESIAN_POINT('Ctrl Pts',(118.779955786451,-121.619960181736,85.394093024668));
#24618=CARTESIAN_POINT('Ctrl Pts',(116.330634260051,-124.011396018777,81.8918489994272));
#24619=CARTESIAN_POINT('Ctrl Pts',(120.526719842212,-125.454244503486,83.9470465127606));
#24620=CARTESIAN_POINT('Ctrl Pts',(118.976188771633,-121.427849190967,85.1007432598139));
#24621=CARTESIAN_POINT('Ctrl Pts',(116.22633468612,-124.12159432885,81.7284336163675));
#24622=CARTESIAN_POINT('Ctrl Pts',(120.725838606435,-125.356776429138,83.8003716291908));
#24623=CARTESIAN_POINT('Ctrl Pts',(119.229508592988,-121.178951530852,84.6051856591982));
#24624=CARTESIAN_POINT('Ctrl Pts',(116.018327623081,-124.338324238802,81.6176595477783));
#24625=CARTESIAN_POINT('Ctrl Pts',(120.982883719393,-125.230497467175,83.5525928299572));
#24626=CARTESIAN_POINT('Ctrl Pts',(119.306430749593,-121.103197399825,84.4313845009826));
#24627=CARTESIAN_POINT('Ctrl Pts',(115.938944698972,-124.420612015483,81.6055951047046));
#24628=CARTESIAN_POINT('Ctrl Pts',(121.060937084102,-125.192063387035,83.4656922503483));
#24629=CARTESIAN_POINT('Ctrl Pts',(119.440303841193,-120.971164568222,84.0733653040093));
#24630=CARTESIAN_POINT('Ctrl Pts',(115.778652442948,-124.586368326784,81.6400246699492));
#24631=CARTESIAN_POINT('Ctrl Pts',(121.196778897725,-125.125076140871,83.2866826521477));
#24632=CARTESIAN_POINT('Ctrl Pts',(119.497839395062,-120.914311737672,83.8880856770355));
#24633=CARTESIAN_POINT('Ctrl Pts',(115.697759348993,-124.669813047928,81.687827278078));
#24634=CARTESIAN_POINT('Ctrl Pts',(121.255160562605,-125.096231691082,83.1940428383536));
#24635=CARTESIAN_POINT('Ctrl Pts',(119.592195409222,-120.820988244119,83.5036466079772));
#24636=CARTESIAN_POINT('Ctrl Pts',(115.551887637631,-124.820142027722,81.8435231238131));
#24637=CARTESIAN_POINT('Ctrl Pts',(121.350904165271,-125.048883740856,83.0018233041528));
#24638=CARTESIAN_POINT('Ctrl Pts',(119.628897626029,-120.784634828299,83.3034927483087));
#24639=CARTESIAN_POINT('Ctrl Pts',(115.488159523431,-124.885734117079,81.9531151909441));
#24640=CARTESIAN_POINT('Ctrl Pts',(121.388146120508,-125.030439729044,82.9017463741549));
#24641=CARTESIAN_POINT('Ctrl Pts',(119.677240002648,-120.736735847766,82.9038841796106));
#24642=CARTESIAN_POINT('Ctrl Pts',(115.400689666877,-124.975740417798,82.2081803578444));
#24643=CARTESIAN_POINT('Ctrl Pts',(121.437199414473,-125.006138040429,82.7019420898048));
#24644=CARTESIAN_POINT('Ctrl Pts',(119.689439202153,-120.724637682099,82.7026620014997));
#24645=CARTESIAN_POINT('Ctrl Pts',(115.37709911597,-124.99999999812,82.3529550603214));
#24646=CARTESIAN_POINT('Ctrl Pts',(121.449578013946,-125.,82.6013310007504));
#24647=CARTESIAN_POINT('Ctrl Pts',(119.689439203101,-120.724637681159,82.5));
#24648=CARTESIAN_POINT('Ctrl Pts',(115.377099114166,-125.,82.5));
#24649=CARTESIAN_POINT('Ctrl Pts',(121.449578014911,-125.,82.5));
#24650=CARTESIAN_POINT('Origin',(152.5,-80.6225774829854,115.));
#24651=CARTESIAN_POINT('Origin',(152.5,-80.6225774829854,-37.5));
#24652=CARTESIAN_POINT('Origin',(147.5,-79.9999999999999,-37.5));
#24653=CARTESIAN_POINT('Origin',(147.5,-122.5,-37.5));
#24654=CARTESIAN_POINT('Ctrl Pts',(147.5,-89.4427190999916,-35.));
#24655=CARTESIAN_POINT('Ctrl Pts',(147.692029124325,-88.8093685907339,-35.));
#24656=CARTESIAN_POINT('Ctrl Pts',(147.88101932576,-88.1768396514604,-35.0215706395705));
#24657=CARTESIAN_POINT('Ctrl Pts',(148.067032922317,-87.5451886182185,-35.0650289615107));
#24658=CARTESIAN_POINT('Ctrl Pts',(148.113199638342,-87.3884191432013,-35.0758148827823));
#24659=CARTESIAN_POINT('Ctrl Pts',(148.159182993898,-87.2317038211986,-35.0879492852677));
#24660=CARTESIAN_POINT('Ctrl Pts',(148.204983936061,-87.0750436647327,-35.1014374973016));
#24661=CARTESIAN_POINT('Ctrl Pts',(148.227650188963,-86.9975147197266,-35.1081126269108));
#24662=CARTESIAN_POINT('Ctrl Pts',(148.250265804086,-86.9200215223735,-35.115117542436));
#24663=CARTESIAN_POINT('Ctrl Pts',(148.272833473781,-86.8425552539345,-35.1224532765259));
#24664=CARTESIAN_POINT('Ctrl Pts',(148.349179005424,-86.5804899397761,-35.1472697740491));
#24665=CARTESIAN_POINT('Ctrl Pts',(148.42497434187,-86.3187382385474,-35.1759312643129));
#24666=CARTESIAN_POINT('Ctrl Pts',(148.500300623548,-86.0570314558247,-35.2088246089286));
#24667=CARTESIAN_POINT('Ctrl Pts',(148.548487711965,-85.8896146180706,-35.2298668596546));
#24668=CARTESIAN_POINT('Ctrl Pts',(148.596482723494,-85.722216299478,-35.2526418166199));
#24669=CARTESIAN_POINT('Ctrl Pts',(148.644305530043,-85.5547679896948,-35.27726185663));
#24670=CARTESIAN_POINT('Ctrl Pts',(148.705029122345,-85.3421484546081,-35.3085234529253));
#24671=CARTESIAN_POINT('Ctrl Pts',(148.765481316966,-85.1294146679281,-35.3427818320588));
#24672=CARTESIAN_POINT('Ctrl Pts',(148.825445173693,-84.9173615302769,-35.3802763718155));
#24673=CARTESIAN_POINT('Ctrl Pts',(148.844370664429,-84.8504343859753,-35.3921102097894));
#24674=CARTESIAN_POINT('Ctrl Pts',(148.863247416419,-84.7835753430873,-35.4042666139058));
#24675=CARTESIAN_POINT('Ctrl Pts',(148.882068323814,-84.716810316948,-35.4167536897875));
#24676=CARTESIAN_POINT('Ctrl Pts',(148.922791444534,-84.5723496827033,-35.4437721904313));
#24677=CARTESIAN_POINT('Ctrl Pts',(148.963298334263,-84.4281714850057,-35.472367305025));
#24678=CARTESIAN_POINT('Ctrl Pts',(149.003534667861,-84.2844711674245,-35.5026558877997));
#24679=CARTESIAN_POINT('Ctrl Pts',(149.04618468002,-84.1321506216861,-35.5347614080625));
#24680=CARTESIAN_POINT('Ctrl Pts',(149.088661184879,-83.9798999175319,-35.5688472728399));
#24681=CARTESIAN_POINT('Ctrl Pts',(149.130874866131,-83.8280577824072,-35.6051699481951));
#24682=CARTESIAN_POINT('Ctrl Pts',(149.153428770922,-83.7469316413739,-35.6245764092618));
#24683=CARTESIAN_POINT('Ctrl Pts',(149.175907457703,-83.6659227740306,-35.6446218401457));
#24684=CARTESIAN_POINT('Ctrl Pts',(149.198295786019,-83.5850879910549,-35.6653487919112));
#24685=CARTESIAN_POINT('Ctrl Pts',(149.227912989617,-83.4781527973521,-35.6927681839146));
#24686=CARTESIAN_POINT('Ctrl Pts',(149.257371929547,-83.3715229731208,-35.7213784236265));
#24687=CARTESIAN_POINT('Ctrl Pts',(149.286670239745,-83.2652102217286,-35.7513256085597));
#24688=CARTESIAN_POINT('Ctrl Pts',(149.305367125227,-83.1973661268101,-35.7704365771927));
#24689=CARTESIAN_POINT('Ctrl Pts',(149.323998297626,-83.1296521688589,-35.7900922411323));
#24690=CARTESIAN_POINT('Ctrl Pts',(149.342561050911,-83.0620783213206,-35.8103347154936));
#24691=CARTESIAN_POINT('Ctrl Pts',(149.371267458519,-82.957578607228,-35.8416387311794));
#24692=CARTESIAN_POINT('Ctrl Pts',(149.399774767598,-82.85354358919,-35.8742597573607));
#24693=CARTESIAN_POINT('Ctrl Pts',(149.428061694082,-82.7500633861336,-35.9084779858677));
#24694=CARTESIAN_POINT('Ctrl Pts',(149.454923581066,-82.6517963113699,-35.9409723675915));
#24695=CARTESIAN_POINT('Ctrl Pts',(149.481586763681,-82.5540293874012,-35.9749069410053));
#24696=CARTESIAN_POINT('Ctrl Pts',(149.508023085916,-82.4568752753899,-36.0105521857167));
#24697=CARTESIAN_POINT('Ctrl Pts',(149.512553176897,-82.4402270834549,-36.0166603046963));
#24698=CARTESIAN_POINT('Ctrl Pts',(149.517076580988,-82.423596977919,-36.0228187343151));
#24699=CARTESIAN_POINT('Ctrl Pts',(149.521593124103,-82.4069856432661,-36.0290289363977));
#24700=CARTESIAN_POINT('Ctrl Pts',(149.546047412518,-82.3170455368108,-36.0626533409432));
#24701=CARTESIAN_POINT('Ctrl Pts',(149.570311794243,-82.2276143985182,-36.0978073544201));
#24702=CARTESIAN_POINT('Ctrl Pts',(149.594353719129,-82.1388178247201,-36.1347461416766));
#24703=CARTESIAN_POINT('Ctrl Pts',(149.612438155904,-82.0720246693327,-36.1625316524403));
#24704=CARTESIAN_POINT('Ctrl Pts',(149.630396548314,-82.0055912015778,-36.1913275605318));
#24705=CARTESIAN_POINT('Ctrl Pts',(149.648211128679,-81.9395854582948,-36.221254932904));
#24706=CARTESIAN_POINT('Ctrl Pts',(149.655934224025,-81.9109702095317,-36.2342292463905));
#24707=CARTESIAN_POINT('Ctrl Pts',(149.663637104736,-81.8824099165127,-36.2474379019951));
#24708=CARTESIAN_POINT('Ctrl Pts',(149.67131055004,-81.8539394834481,-36.2608852437837));
#24709=CARTESIAN_POINT('Ctrl Pts',(149.685698655412,-81.800555954318,-36.2860997026037));
#24710=CARTESIAN_POINT('Ctrl Pts',(149.699999360784,-81.7474243598168,-36.3121788856479));
#24711=CARTESIAN_POINT('Ctrl Pts',(149.714175605293,-81.6946906272435,-36.3392201558046));
#24712=CARTESIAN_POINT('Ctrl Pts',(149.727286670728,-81.6459192182899,-36.3642295905834));
#24713=CARTESIAN_POINT('Ctrl Pts',(149.7402913331,-81.5974878782028,-36.3900621045965));
#24714=CARTESIAN_POINT('Ctrl Pts',(149.753148950424,-81.5495528039874,-36.4168048599215));
#24715=CARTESIAN_POINT('Ctrl Pts',(149.762929820709,-81.5130882918453,-36.4371482419277));
#24716=CARTESIAN_POINT('Ctrl Pts',(149.7726254041,-81.4769116545467,-36.4580185544263));
#24717=CARTESIAN_POINT('Ctrl Pts',(149.782212501331,-81.4411109947047,-36.4794579384386));
#24718=CARTESIAN_POINT('Ctrl Pts',(149.792712453297,-81.4019015030661,-36.502938716499));
#24719=CARTESIAN_POINT('Ctrl Pts',(149.80309231573,-81.3631061432707,-36.5271022623885));
#24720=CARTESIAN_POINT('Ctrl Pts',(149.813325028167,-81.3248298095057,-36.5520580116851));
#24721=CARTESIAN_POINT('Ctrl Pts',(149.822817814989,-81.2893212306252,-36.57520921519));
#24722=CARTESIAN_POINT('Ctrl Pts',(149.832167251567,-81.2543175533125,-36.5989995466143));
#24723=CARTESIAN_POINT('Ctrl Pts',(149.841373631762,-81.2198208405048,-36.6235944717091));
#24724=CARTESIAN_POINT('Ctrl Pts',(149.850444720925,-81.1858310691643,-36.6478279656298));
#24725=CARTESIAN_POINT('Ctrl Pts',(149.859377062135,-81.1523329411813,-36.6728423498981));
#24726=CARTESIAN_POINT('Ctrl Pts',(149.868158592941,-81.1193744240766,-36.6988172833898));
#24727=CARTESIAN_POINT('Ctrl Pts',(149.876313696669,-81.0887669899474,-36.7229393051219));
#24728=CARTESIAN_POINT('Ctrl Pts',(149.884338741475,-81.0586248955809,-36.7478897210516));
#24729=CARTESIAN_POINT('Ctrl Pts',(149.892212585395,-81.0290296767013,-36.7738322591383));
#24730=CARTESIAN_POINT('Ctrl Pts',(149.89281740775,-81.0267563461447,-36.7758250122512));
#24731=CARTESIAN_POINT('Ctrl Pts',(149.89342133192,-81.0244862651392,-36.7778236297116));
#24732=CARTESIAN_POINT('Ctrl Pts',(149.894024345238,-81.0222194822742,-36.7798281910486));
#24733=CARTESIAN_POINT('Ctrl Pts',(149.901678691384,-80.9934460867893,-36.805273079051));
#24734=CARTESIAN_POINT('Ctrl Pts',(149.909127380051,-80.9654260581732,-36.8314799870868));
#24735=CARTESIAN_POINT('Ctrl Pts',(149.916327644768,-80.9383234966228,-36.8585857768089));
#24736=CARTESIAN_POINT('Ctrl Pts',(149.922896825409,-80.9135964026002,-36.8833158160625));
#24737=CARTESIAN_POINT('Ctrl Pts',(149.929259164437,-80.8896331987156,-36.9087941212806));
#24738=CARTESIAN_POINT('Ctrl Pts',(149.935369835439,-80.8666055523399,-36.9351356817967));
#24739=CARTESIAN_POINT('Ctrl Pts',(149.935956871689,-80.8643933463218,-36.9376662469162));
#24740=CARTESIAN_POINT('Ctrl Pts',(149.936541575424,-80.8621898122598,-36.9402047878345));
#24741=CARTESIAN_POINT('Ctrl Pts',(149.937123900464,-80.8599951269442,-36.9427514122747));
#24742=CARTESIAN_POINT('Ctrl Pts',(149.949888621083,-80.8118870379003,-36.9985741010473));
#24743=CARTESIAN_POINT('Ctrl Pts',(149.961572072671,-80.7677918263995,-37.0585526832355));
#24744=CARTESIAN_POINT('Ctrl Pts',(149.971367310254,-80.7307169524392,-37.1227154597912));
#24745=CARTESIAN_POINT('Ctrl Pts',(149.975158206732,-80.7163684480826,-37.1475473683212));
#24746=CARTESIAN_POINT('Ctrl Pts',(149.978650998302,-80.7031305919437,-37.1730908787877));
#24747=CARTESIAN_POINT('Ctrl Pts',(149.981796037926,-80.6911891223571,-37.1992286595142));
#24748=CARTESIAN_POINT('Ctrl Pts',(149.985757876154,-80.6761463323226,-37.2321546862971));
#24749=CARTESIAN_POINT('Ctrl Pts',(149.989179977686,-80.6631984113666,-37.2661215533609));
#24750=CARTESIAN_POINT('Ctrl Pts',(149.991954976261,-80.6527310533642,-37.3008958029158));
#24751=CARTESIAN_POINT('Ctrl Pts',(149.993127423005,-80.6483085574699,-37.3155880467322));
#24752=CARTESIAN_POINT('Ctrl Pts',(149.994184300917,-80.6443291875707,-37.33042386883));
#24753=CARTESIAN_POINT('Ctrl Pts',(149.995117265699,-80.6408234431072,-37.3453832597703));
#24754=CARTESIAN_POINT('Ctrl Pts',(149.997168971269,-80.633113875098,-37.3782808206258));
#24755=CARTESIAN_POINT('Ctrl Pts',(149.998622294846,-80.6276965661506,-37.4117792041177));
#24756=CARTESIAN_POINT('Ctrl Pts',(149.999384955835,-80.6248606269893,-37.4456825897633));
#24757=CARTESIAN_POINT('Ctrl Pts',(149.999789923498,-80.6233547630873,-37.4636850509217));
#24758=CARTESIAN_POINT('Ctrl Pts',(150.,-80.6225774829854,-37.4818014034218));
#24759=CARTESIAN_POINT('Ctrl Pts',(150.,-80.6225774829854,-37.5));
#24760=CARTESIAN_POINT('Origin',(152.5,-122.5,85.));
#24761=CARTESIAN_POINT('Origin',(152.5,-122.5,-37.5));
#24762=CARTESIAN_POINT('Origin',(0.,-122.5,49.5));
#24763=CARTESIAN_POINT('Origin',(121.449578014911,-122.5,49.5));
#24764=CARTESIAN_POINT('Origin',(147.5,-122.5,49.5));
#24765=CARTESIAN_POINT('Ctrl Pts',(145.36231884058,-88.1464478086873,-32.5));
#24766=CARTESIAN_POINT('Ctrl Pts',(145.36231884058,-88.1464478086873,-35.));
#24767=CARTESIAN_POINT('Ctrl Pts',(147.5,-89.4427190999916,-35.));
#24768=CARTESIAN_POINT('Ctrl Pts',(145.883280419022,-87.287330000178,-32.5000000009303));
#24769=CARTESIAN_POINT('Ctrl Pts',(145.793011707107,-87.4361921450692,-34.7836438007554));
#24770=CARTESIAN_POINT('Ctrl Pts',(147.764311380885,-88.5709672327977,-35.));
#24771=CARTESIAN_POINT('Ctrl Pts',(146.390924783416,-86.4329953777441,-32.5817470282946));
#24772=CARTESIAN_POINT('Ctrl Pts',(146.256366271119,-86.6602829701324,-34.6533815799968));
#24773=CARTESIAN_POINT('Ctrl Pts',(148.021866250328,-87.7040688391623,-35.0408735143647));
#24774=CARTESIAN_POINT('Ctrl Pts',(147.132955592072,-85.159466684389,-32.8264997589554));
#24775=CARTESIAN_POINT('Ctrl Pts',(146.95625485105,-85.4644664729262,-34.6060350541333));
#24776=CARTESIAN_POINT('Ctrl Pts',(148.398337763665,-86.4118117826985,-35.163249879369));
#24777=CARTESIAN_POINT('Ctrl Pts',(147.377049426154,-84.7363019818542,-32.9287776457782));
#24778=CARTESIAN_POINT('Ctrl Pts',(147.185340564392,-85.0695699101127,-34.6128471107274));
#24779=CARTESIAN_POINT('Ctrl Pts',(148.522179488132,-85.9824240698147,-35.2143888231312));
#24780=CARTESIAN_POINT('Ctrl Pts',(147.858493843555,-83.8933928830767,-33.1802802395072));
#24781=CARTESIAN_POINT('Ctrl Pts',(147.640340054158,-84.2776371924664,-34.6763398436954));
#24782=CARTESIAN_POINT('Ctrl Pts',(148.766441729588,-85.1271192490123,-35.3401401195115));
#24783=CARTESIAN_POINT('Ctrl Pts',(148.095887496715,-83.473525962111,-33.3296903827866));
#24784=CARTESIAN_POINT('Ctrl Pts',(147.866955151253,-83.8795640251386,-34.7317798844392));
#24785=CARTESIAN_POINT('Ctrl Pts',(148.886884097339,-84.701077814479,-35.4148451917191));
#24786=CARTESIAN_POINT('Ctrl Pts',(148.555727425866,-82.6523882229576,-33.6809331684121));
#24787=CARTESIAN_POINT('Ctrl Pts',(148.307824862021,-83.0977615436452,-34.8965208417471));
#24788=CARTESIAN_POINT('Ctrl Pts',(149.120185238382,-83.86786452037,-35.5904665838802));
#24789=CARTESIAN_POINT('Ctrl Pts',(148.780093861297,-82.2476812683578,-33.8839399244688));
#24790=CARTESIAN_POINT('Ctrl Pts',(148.52472777307,-82.7095240936269,-35.0050364952419));
#24791=CARTESIAN_POINT('Ctrl Pts',(149.234018208523,-83.4572059928576,-35.69196996268));
#24792=CARTESIAN_POINT('Ctrl Pts',(149.207972890121,-81.4688789012016,-34.3573989375057));
#24793=CARTESIAN_POINT('Ctrl Pts',(148.939317285436,-81.9607628458189,-35.2860875789416));
#24794=CARTESIAN_POINT('Ctrl Pts',(149.451103893298,-82.6669506497836,-35.9286994683073));
#24795=CARTESIAN_POINT('Ctrl Pts',(149.410469407752,-81.0966396786722,-34.6254381321728));
#24796=CARTESIAN_POINT('Ctrl Pts',(149.13707735126,-81.6002642788733,-35.4559386647908));
#24797=CARTESIAN_POINT('Ctrl Pts',(149.553841095111,-82.2892373209608,-36.0627190669335));
#24798=CARTESIAN_POINT('Ctrl Pts',(149.689478100498,-80.5797647052594,-35.1010485304976));
#24799=CARTESIAN_POINT('Ctrl Pts',(149.410828634125,-81.0973762069276,-35.7764659917703));
#24800=CARTESIAN_POINT('Ctrl Pts',(149.695396978193,-81.7647612450649,-36.3005242648253));
#24801=CARTESIAN_POINT('Ctrl Pts',(149.778860900692,-80.4134491496523,-35.2734504935361));
#24802=CARTESIAN_POINT('Ctrl Pts',(149.498351131334,-80.9359152801443,-35.8944893614086));
#24803=CARTESIAN_POINT('Ctrl Pts',(149.740745603139,-81.595999872402,-36.3867252471501));
#24804=CARTESIAN_POINT('Ctrl Pts',(149.942345818683,-80.1081950067719,-35.6444293836609));
#24805=CARTESIAN_POINT('Ctrl Pts',(149.65844369221,-80.6395711160561,-36.153254701076));
#24806=CARTESIAN_POINT('Ctrl Pts',(149.823690158897,-81.2862566980873,-36.5722146914484));
#24807=CARTESIAN_POINT('Ctrl Pts',(150.016754772459,-79.9686937648418,-35.8430315532085));
#24808=CARTESIAN_POINT('Ctrl Pts',(149.731542660712,-80.5037270542566,-36.2939840338164));
#24809=CARTESIAN_POINT('Ctrl Pts',(149.861441758745,-81.144703967216,-36.6715157768338));
#24810=CARTESIAN_POINT('Ctrl Pts',(150.145196691125,-79.7272764209246,-36.2762826327136));
#24811=CARTESIAN_POINT('Ctrl Pts',(149.857607243134,-80.2688649285009,-36.6048325581329));
#24812=CARTESIAN_POINT('Ctrl Pts',(149.926607145573,-80.8997363683411,-36.8881413161273));
#24813=CARTESIAN_POINT('Ctrl Pts',(150.197080555724,-79.6294105444985,-36.5038809199123));
#24814=CARTESIAN_POINT('Ctrl Pts',(149.908727602392,-80.1732994372084,-36.7701162187303));
#24815=CARTESIAN_POINT('Ctrl Pts',(149.952930574586,-80.8004312877628,-37.0019404601773));
#24816=CARTESIAN_POINT('Ctrl Pts',(150.269771338359,-79.4921496315481,-36.9870649844503));
#24817=CARTESIAN_POINT('Ctrl Pts',(149.980179574577,-80.0395829024242,-37.1229099719677));
#24818=CARTESIAN_POINT('Ctrl Pts',(149.989810459912,-80.6611518320492,-37.243532492004));
#24819=CARTESIAN_POINT('Ctrl Pts',(150.289855071895,-79.4541343321333,-37.2465705504854));
#24820=CARTESIAN_POINT('Ctrl Pts',(149.99999999943,-80.0024038110911,-37.313811727788));
#24821=CARTESIAN_POINT('Ctrl Pts',(150.,-80.6225774840775,-37.3732852754135));
#24822=CARTESIAN_POINT('Ctrl Pts',(150.289855072464,-79.4541343310581,-37.5));
#24823=CARTESIAN_POINT('Ctrl Pts',(150.,-80.0024038100394,-37.5));
#24824=CARTESIAN_POINT('Ctrl Pts',(150.,-80.6225774829855,-37.5));
#24825=CARTESIAN_POINT('Origin',(147.5,-89.4427190999916,-32.5));
#24826=CARTESIAN_POINT('Origin',(147.5,-122.5,-37.5));
#24827=CARTESIAN_POINT('Origin',(147.5,-122.5,-32.5));
#24828=CARTESIAN_POINT('Origin',(147.5,-122.5,44.5));
#24829=CARTESIAN_POINT('Origin',(152.5,-122.5,44.5));
#24830=CARTESIAN_POINT('Origin',(147.5,-122.5,44.5));
#24831=CARTESIAN_POINT('Origin',(121.449578014911,-122.5,49.5));
#24832=CARTESIAN_POINT('Origin',(121.449578014911,-122.5,49.5));
#24833=CARTESIAN_POINT('Origin',(0.,0.,-32.5));
#24834=CARTESIAN_POINT('Origin',(121.449578014911,-122.5,-32.5));
#24835=CARTESIAN_POINT('Origin',(0.,-122.5,-32.5));
#24836=CARTESIAN_POINT('Origin',(121.449578014911,-122.5,-32.5));
#24837=CARTESIAN_POINT('Origin',(152.5,-122.5,47.));
#24838=CARTESIAN_POINT('Origin',(152.5,-122.5,37.5));
#24839=CARTESIAN_POINT('Origin',(147.5,-79.9999999999999,44.5));
#24840=CARTESIAN_POINT('Ctrl Pts',(147.5,-89.4427190999916,47.));
#24841=CARTESIAN_POINT('Ctrl Pts',(147.692029124167,-88.8093685912607,47.));
#24842=CARTESIAN_POINT('Ctrl Pts',(147.881019325447,-88.1768396525117,46.9784293604652));
#24843=CARTESIAN_POINT('Ctrl Pts',(148.067032921855,-87.5451886197927,46.9349710385975));
#24844=CARTESIAN_POINT('Ctrl Pts',(148.113199638035,-87.3884191442505,46.9241851172987));
#24845=CARTESIAN_POINT('Ctrl Pts',(148.159182993745,-87.2317038217232,46.9120507147773));
#24846=CARTESIAN_POINT('Ctrl Pts',(148.204983936061,-87.075043664733,46.8985625026983));
#24847=CARTESIAN_POINT('Ctrl Pts',(148.227650188964,-86.9975147197269,46.8918873730891));
#24848=CARTESIAN_POINT('Ctrl Pts',(148.250265804087,-86.9200215223737,46.8848824575639));
#24849=CARTESIAN_POINT('Ctrl Pts',(148.272833473781,-86.8425552539348,46.877546723474));
#24850=CARTESIAN_POINT('Ctrl Pts',(148.349179005414,-86.5804899398113,46.8527302259542));
#24851=CARTESIAN_POINT('Ctrl Pts',(148.42497434185,-86.3187382386177,46.8240687356948));
#24852=CARTESIAN_POINT('Ctrl Pts',(148.500300623518,-86.0570314559301,46.7911753910845));
#24853=CARTESIAN_POINT('Ctrl Pts',(148.548487711945,-85.8896146181409,46.7701331403549));
#24854=CARTESIAN_POINT('Ctrl Pts',(148.596482723484,-85.7222162995132,46.7473581833852));
#24855=CARTESIAN_POINT('Ctrl Pts',(148.644305530043,-85.5547679896948,46.7227381433699));
#24856=CARTESIAN_POINT('Ctrl Pts',(148.705029122316,-85.3421484547092,46.6914765470896));
#24857=CARTESIAN_POINT('Ctrl Pts',(148.765481316907,-85.1294146681287,46.6572181679748));
#24858=CARTESIAN_POINT('Ctrl Pts',(148.825445173605,-84.9173615305767,46.6197236282395));
#24859=CARTESIAN_POINT('Ctrl Pts',(148.844370664369,-84.8504343861742,46.6078897902489));
#24860=CARTESIAN_POINT('Ctrl Pts',(148.863247416388,-84.7835753431854,46.5957333861149));
#24861=CARTESIAN_POINT('Ctrl Pts',(148.882068323811,-84.7168103169457,46.5832463102145));
#24862=CARTESIAN_POINT('Ctrl Pts',(148.922791444531,-84.5723496827009,46.5562278095707));
#24863=CARTESIAN_POINT('Ctrl Pts',(148.963298334261,-84.4281714850036,46.5276326949765));
#24864=CARTESIAN_POINT('Ctrl Pts',(149.003534667861,-84.2844711674245,46.4973441122003));
#24865=CARTESIAN_POINT('Ctrl Pts',(149.04618468001,-84.1321506217299,46.4652385919447));
#24866=CARTESIAN_POINT('Ctrl Pts',(149.088661184858,-83.9798999176171,46.431152727177));
#24867=CARTESIAN_POINT('Ctrl Pts',(149.130874866099,-83.8280577825329,46.3948300518332));
#24868=CARTESIAN_POINT('Ctrl Pts',(149.153428770871,-83.7469316415657,46.3754235907832));
#24869=CARTESIAN_POINT('Ctrl Pts',(149.175907457634,-83.6659227742882,46.3553781599173));
#24870=CARTESIAN_POINT('Ctrl Pts',(149.198295785931,-83.5850879913779,46.3346512081709));
#24871=CARTESIAN_POINT('Ctrl Pts',(149.227912989408,-83.4781527981097,46.3072318162821));
#24872=CARTESIAN_POINT('Ctrl Pts',(149.257371929218,-83.3715229743104,46.2786215766946));
#24873=CARTESIAN_POINT('Ctrl Pts',(149.286670239298,-83.265210223348,46.2486743918971));
#24874=CARTESIAN_POINT('Ctrl Pts',(149.30536712493,-83.1973661278873,46.2295634231207));
#24875=CARTESIAN_POINT('Ctrl Pts',(149.323998297478,-83.1296521693962,46.2099077590292));
#24876=CARTESIAN_POINT('Ctrl Pts',(149.342561050911,-83.0620783213206,46.1896652845064));
#24877=CARTESIAN_POINT('Ctrl Pts',(149.371267458519,-82.95757860723,46.1583612688204));
#24878=CARTESIAN_POINT('Ctrl Pts',(149.399774767598,-82.8535435891935,46.1257402426392));
#24879=CARTESIAN_POINT('Ctrl Pts',(149.428061694081,-82.7500633861384,46.0915220141326));
#24880=CARTESIAN_POINT('Ctrl Pts',(149.454923581065,-82.6517963113774,46.0590276324095));
#24881=CARTESIAN_POINT('Ctrl Pts',(149.48158676368,-82.5540293874111,46.0250930589968));
#24882=CARTESIAN_POINT('Ctrl Pts',(149.508023085913,-82.4568752754022,45.9894478142867));
#24883=CARTESIAN_POINT('Ctrl Pts',(149.512553176896,-82.4402270834634,45.9833396953057));
#24884=CARTESIAN_POINT('Ctrl Pts',(149.517076580988,-82.4235969779237,45.9771812656855));
#24885=CARTESIAN_POINT('Ctrl Pts',(149.521593124104,-82.406985643267,45.9709710636017));
#24886=CARTESIAN_POINT('Ctrl Pts',(149.546047412515,-82.3170455368253,45.9373466590614));
#24887=CARTESIAN_POINT('Ctrl Pts',(149.570311794236,-82.2276143985462,45.9021926455905));
#24888=CARTESIAN_POINT('Ctrl Pts',(149.594353719118,-82.1388178247614,45.8652538583403));
#24889=CARTESIAN_POINT('Ctrl Pts',(149.612438155897,-82.07202466936,45.8374683475715));
#24890=CARTESIAN_POINT('Ctrl Pts',(149.63039654831,-82.0055912015912,45.8086724394745));
#24891=CARTESIAN_POINT('Ctrl Pts',(149.648211128679,-81.9395854582945,45.7787450670962));
#24892=CARTESIAN_POINT('Ctrl Pts',(149.655934224025,-81.9109702095313,45.7657707536098));
#24893=CARTESIAN_POINT('Ctrl Pts',(149.663637104736,-81.8824099165123,45.7525620980052));
#24894=CARTESIAN_POINT('Ctrl Pts',(149.67131055004,-81.8539394834478,45.7391147562166));
#24895=CARTESIAN_POINT('Ctrl Pts',(149.685698655415,-81.8005559543078,45.7139002973917));
#24896=CARTESIAN_POINT('Ctrl Pts',(149.699999360789,-81.7474243597972,45.6878211143421));
#24897=CARTESIAN_POINT('Ctrl Pts',(149.714175605301,-81.6946906272146,45.6607798441796));
#24898=CARTESIAN_POINT('Ctrl Pts',(149.727286670739,-81.6459192182512,45.6357704093948));
#24899=CARTESIAN_POINT('Ctrl Pts',(149.740291333114,-81.5974878781543,45.6099378953754));
#24900=CARTESIAN_POINT('Ctrl Pts',(149.75314895044,-81.549552803929,45.583195140044));
#24901=CARTESIAN_POINT('Ctrl Pts',(149.76292982072,-81.5130882918071,45.5628517580484));
#24902=CARTESIAN_POINT('Ctrl Pts',(149.772625404106,-81.4769116545282,45.5419814455611));
#24903=CARTESIAN_POINT('Ctrl Pts',(149.782212501331,-81.4411109947051,45.5205420615612));
#24904=CARTESIAN_POINT('Ctrl Pts',(149.792712453297,-81.4019015030656,45.4970612835013));
#24905=CARTESIAN_POINT('Ctrl Pts',(149.80309231573,-81.3631061432697,45.4728977376122));
#24906=CARTESIAN_POINT('Ctrl Pts',(149.813325028167,-81.3248298095044,45.4479419883158));
#24907=CARTESIAN_POINT('Ctrl Pts',(149.822817814989,-81.2893212306204,45.4247907848088));
#24908=CARTESIAN_POINT('Ctrl Pts',(149.832167251568,-81.2543175533045,45.4010004533823));
#24909=CARTESIAN_POINT('Ctrl Pts',(149.841373631764,-81.2198208404939,45.3764055282848));
#24910=CARTESIAN_POINT('Ctrl Pts',(149.850444720927,-81.1858310691553,45.352172034365));
#24911=CARTESIAN_POINT('Ctrl Pts',(149.859377062136,-81.1523329411743,45.3271576500975));
#24912=CARTESIAN_POINT('Ctrl Pts',(149.868158592942,-81.1193744240714,45.3011827166068));
#24913=CARTESIAN_POINT('Ctrl Pts',(149.876313696672,-81.0887669899374,45.2770606948705));
#24914=CARTESIAN_POINT('Ctrl Pts',(149.884338741479,-81.0586248955663,45.2521102789363));
#24915=CARTESIAN_POINT('Ctrl Pts',(149.8922125854,-81.0290296766821,45.2261677408448));
#24916=CARTESIAN_POINT('Ctrl Pts',(149.892817407753,-81.0267563461319,45.2241749877375));
#24917=CARTESIAN_POINT('Ctrl Pts',(149.893421331922,-81.0244862651328,45.2221763702828));
#24918=CARTESIAN_POINT('Ctrl Pts',(149.894024345238,-81.0222194822742,45.2201718089514));
#24919=CARTESIAN_POINT('Ctrl Pts',(149.901678691384,-80.9934460867894,45.194726920949));
#24920=CARTESIAN_POINT('Ctrl Pts',(149.909127380051,-80.9654260581732,45.1685200129132));
#24921=CARTESIAN_POINT('Ctrl Pts',(149.916327644768,-80.9383234966228,45.1414142231911));
#24922=CARTESIAN_POINT('Ctrl Pts',(149.922896825408,-80.9135964026004,45.1166841839377));
#24923=CARTESIAN_POINT('Ctrl Pts',(149.929259164437,-80.8896331987158,45.0912058787197));
#24924=CARTESIAN_POINT('Ctrl Pts',(149.935369835439,-80.8666055523403,45.0648643182037));
#24925=CARTESIAN_POINT('Ctrl Pts',(149.935956871689,-80.864393346322,45.0623337530841));
#24926=CARTESIAN_POINT('Ctrl Pts',(149.936541575424,-80.8621898122599,45.0597952121657));
#24927=CARTESIAN_POINT('Ctrl Pts',(149.937123900464,-80.8599951269442,45.0572485877254));
#24928=CARTESIAN_POINT('Ctrl Pts',(149.949888621083,-80.8118870379003,45.0014258989527));
#24929=CARTESIAN_POINT('Ctrl Pts',(149.961572072671,-80.7677918263995,44.9414473167645));
#24930=CARTESIAN_POINT('Ctrl Pts',(149.971367310254,-80.7307169524392,44.8772845402088));
#24931=CARTESIAN_POINT('Ctrl Pts',(149.975158206732,-80.7163684480826,44.8524526316788));
#24932=CARTESIAN_POINT('Ctrl Pts',(149.978650998302,-80.7031305919437,44.8269091212123));
#24933=CARTESIAN_POINT('Ctrl Pts',(149.981796037926,-80.6911891223571,44.8007713404859));
#24934=CARTESIAN_POINT('Ctrl Pts',(149.985757876155,-80.6761463323222,44.767845313702));
#24935=CARTESIAN_POINT('Ctrl Pts',(149.989179977686,-80.6631984113658,44.7338784466372));
#24936=CARTESIAN_POINT('Ctrl Pts',(149.991954976262,-80.6527310533633,44.6991041970813));
#24937=CARTESIAN_POINT('Ctrl Pts',(149.993127423005,-80.6483085574693,44.6844119532658));
#24938=CARTESIAN_POINT('Ctrl Pts',(149.994184300917,-80.6443291875704,44.669576131169));
#24939=CARTESIAN_POINT('Ctrl Pts',(149.995117265699,-80.6408234431072,44.6546167402297));
#24940=CARTESIAN_POINT('Ctrl Pts',(149.997168971269,-80.6331138750976,44.6217191793725));
#24941=CARTESIAN_POINT('Ctrl Pts',(149.998622294847,-80.62769656615,44.5882207958789));
#24942=CARTESIAN_POINT('Ctrl Pts',(149.999384955835,-80.6248606269888,44.5543174102316));
#24943=CARTESIAN_POINT('Ctrl Pts',(149.999789923498,-80.6233547630872,44.5363149490749));
#24944=CARTESIAN_POINT('Ctrl Pts',(150.,-80.6225774829854,44.5181985965764));
#24945=CARTESIAN_POINT('Ctrl Pts',(150.,-80.6225774829854,44.5));
#24946=CARTESIAN_POINT('Origin',(0.,0.,49.5));
#24947=CARTESIAN_POINT('Origin',(147.5,-89.4427190999916,49.5));
#24948=CARTESIAN_POINT('Origin',(121.449578014911,-122.5,-32.5));
#24949=CARTESIAN_POINT('Origin',(147.5,-122.5,37.5));
#24950=CARTESIAN_POINT('Origin',(147.5,-122.5,32.5));
#24951=CARTESIAN_POINT('Origin',(147.5,-122.5,37.5));
#24952=CARTESIAN_POINT('Ctrl Pts',(145.36231884058,-88.1464478086873,49.5));
#24953=CARTESIAN_POINT('Ctrl Pts',(145.36231884058,-88.1464478086873,47.));
#24954=CARTESIAN_POINT('Ctrl Pts',(147.5,-89.4427190999916,47.));
#24955=CARTESIAN_POINT('Ctrl Pts',(145.88328041902,-87.2873300001825,49.4999999990697));
#24956=CARTESIAN_POINT('Ctrl Pts',(145.793011707092,-87.4361921450511,47.2163561992337));
#24957=CARTESIAN_POINT('Ctrl Pts',(147.764311380887,-88.5709672327986,47.));
#24958=CARTESIAN_POINT('Ctrl Pts',(146.390924783419,-86.432995377738,49.4182529717019));
#24959=CARTESIAN_POINT('Ctrl Pts',(146.25636627112,-86.6602829701382,47.3466184200069));
#24960=CARTESIAN_POINT('Ctrl Pts',(148.021866250329,-87.7040688391623,46.959126485635));
#24961=CARTESIAN_POINT('Ctrl Pts',(147.13295559207,-85.1594666843921,49.1735002410464));
#24962=CARTESIAN_POINT('Ctrl Pts',(146.95625485105,-85.4644664729224,47.393964945865));
#24963=CARTESIAN_POINT('Ctrl Pts',(148.398337763665,-86.4118117826985,46.8367501206312));
#24964=CARTESIAN_POINT('Ctrl Pts',(147.377049426154,-84.7363019818542,49.0712223542218));
#24965=CARTESIAN_POINT('Ctrl Pts',(147.185340564392,-85.0695699101127,47.3871528892726));
#24966=CARTESIAN_POINT('Ctrl Pts',(148.522179488132,-85.9824240698147,46.7856111768689));
#24967=CARTESIAN_POINT('Ctrl Pts',(147.858493843555,-83.8933928830767,48.8197197604928));
#24968=CARTESIAN_POINT('Ctrl Pts',(147.640340054158,-84.2776371924664,47.3236601563046));
#24969=CARTESIAN_POINT('Ctrl Pts',(148.766441729588,-85.1271192490123,46.6598598804885));
#24970=CARTESIAN_POINT('Ctrl Pts',(148.095887496716,-83.4735259621086,48.670309617217));
#24971=CARTESIAN_POINT('Ctrl Pts',(147.866955151253,-83.8795640251351,47.2682201155608));
#24972=CARTESIAN_POINT('Ctrl Pts',(148.886884097334,-84.7010778144719,46.5851548082849));
#24973=CARTESIAN_POINT('Ctrl Pts',(148.555727425865,-82.65238822296,48.3190668315844));
#24974=CARTESIAN_POINT('Ctrl Pts',(148.307824862021,-83.0977615436487,47.1034791582529));
#24975=CARTESIAN_POINT('Ctrl Pts',(149.120185238387,-83.867864520377,46.4095334161157));
#24976=CARTESIAN_POINT('Ctrl Pts',(148.780093861296,-82.2476812683581,48.1160600755383));
#24977=CARTESIAN_POINT('Ctrl Pts',(148.524727773055,-82.7095240936236,46.9949635047617));
#24978=CARTESIAN_POINT('Ctrl Pts',(149.234018208522,-83.457205992854,46.308030037322));
#24979=CARTESIAN_POINT('Ctrl Pts',(149.207972890121,-81.4688789012013,47.6426010624872));
#24980=CARTESIAN_POINT('Ctrl Pts',(148.93931728545,-81.9607628458225,46.713912421055));
#24981=CARTESIAN_POINT('Ctrl Pts',(149.4511038933,-82.6669506497871,46.0713005316908));
#24982=CARTESIAN_POINT('Ctrl Pts',(149.410469407752,-81.0966396786721,47.3745618678272));
#24983=CARTESIAN_POINT('Ctrl Pts',(149.13707735126,-81.6002642788733,46.5440613352092));
#24984=CARTESIAN_POINT('Ctrl Pts',(149.553841095111,-82.2892373209608,45.9372809330665));
#24985=CARTESIAN_POINT('Ctrl Pts',(149.689478100498,-80.5797647052593,46.8989514695024));
#24986=CARTESIAN_POINT('Ctrl Pts',(149.410828634125,-81.0973762069276,46.2235340082297));
#24987=CARTESIAN_POINT('Ctrl Pts',(149.695396978193,-81.7647612450649,45.6994757351747));
#24988=CARTESIAN_POINT('Ctrl Pts',(149.778860900691,-80.4134491496535,46.7265495064604));
#24989=CARTESIAN_POINT('Ctrl Pts',(149.498351131341,-80.935915280146,46.1055106385897));
#24990=CARTESIAN_POINT('Ctrl Pts',(149.74074560314,-81.5959998724055,45.6132747528471));
#24991=CARTESIAN_POINT('Ctrl Pts',(149.942345818684,-80.1081950067706,46.3555706163427));
#24992=CARTESIAN_POINT('Ctrl Pts',(149.658443692203,-80.6395711160542,45.8467452989258));
#24993=CARTESIAN_POINT('Ctrl Pts',(149.823690158896,-81.2862566980837,45.4277853085544));
#24994=CARTESIAN_POINT('Ctrl Pts',(150.016754772459,-79.9686937648418,46.1569684467915));
#24995=CARTESIAN_POINT('Ctrl Pts',(149.731542660712,-80.5037270542566,45.7060159661836));
#24996=CARTESIAN_POINT('Ctrl Pts',(149.861441758745,-81.144703967216,45.3284842231662));
#24997=CARTESIAN_POINT('Ctrl Pts',(150.145196691125,-79.7272764209246,45.7237173672864));
#24998=CARTESIAN_POINT('Ctrl Pts',(149.857607243134,-80.2688649285009,45.3951674418671));
#24999=CARTESIAN_POINT('Ctrl Pts',(149.926607145573,-80.8997363683411,45.1118586838727));
#25000=CARTESIAN_POINT('Ctrl Pts',(150.197080555724,-79.6294105444985,45.4961190800877));
#25001=CARTESIAN_POINT('Ctrl Pts',(149.908727602392,-80.1732994372084,45.2298837812697));
#25002=CARTESIAN_POINT('Ctrl Pts',(149.952930574586,-80.8004312877628,44.9980595398227));
#25003=CARTESIAN_POINT('Ctrl Pts',(150.269771338359,-79.4921496315481,45.0129350155497));
#25004=CARTESIAN_POINT('Ctrl Pts',(149.980179574577,-80.0395829024242,44.8770900280323));
#25005=CARTESIAN_POINT('Ctrl Pts',(149.989810459912,-80.6611518320492,44.756467507996));
#25006=CARTESIAN_POINT('Ctrl Pts',(150.289855071895,-79.4541343321333,44.7534294495147));
#25007=CARTESIAN_POINT('Ctrl Pts',(149.99999999943,-80.0024038110911,44.686188272212));
#25008=CARTESIAN_POINT('Ctrl Pts',(150.,-80.6225774840775,44.6267147245865));
#25009=CARTESIAN_POINT('Ctrl Pts',(150.289855072464,-79.4541343310581,44.5));
#25010=CARTESIAN_POINT('Ctrl Pts',(150.,-80.0024038100394,44.5));
#25011=CARTESIAN_POINT('Ctrl Pts',(150.,-80.6225774829855,44.5));
#25012=CARTESIAN_POINT('Origin',(152.5,-80.6225774829854,44.5));
#25013=CARTESIAN_POINT('Origin',(115.217186218029,-122.5,32.5));
#25014=CARTESIAN_POINT('Origin',(121.449578014911,-122.5,32.5));
#25015=CARTESIAN_POINT('Origin',(147.5,0.,37.5));
#25016=CARTESIAN_POINT('Ctrl Pts',(150.,-80.6225774829854,37.5));
#25017=CARTESIAN_POINT('Ctrl Pts',(150.,-80.6225774829854,37.4687656111694));
#25018=CARTESIAN_POINT('Ctrl Pts',(149.999418286665,-80.6247797743348,37.4378789835208));
#25019=CARTESIAN_POINT('Ctrl Pts',(149.998293554945,-80.6290354954266,37.407427664437));
#25020=CARTESIAN_POINT('Ctrl Pts',(149.997125538082,-80.6334549973543,37.3758044305616));
#25021=CARTESIAN_POINT('Ctrl Pts',(149.995371936956,-80.6400888791783,37.3446506435412));
#25022=CARTESIAN_POINT('Ctrl Pts',(149.993090530187,-80.6487160556982,37.3140587875661));
#25023=CARTESIAN_POINT('Ctrl Pts',(149.992231155702,-80.6519657941863,37.3025352570628));
#25024=CARTESIAN_POINT('Ctrl Pts',(149.991297028852,-80.6554978429528,37.2910914065902));
#25025=CARTESIAN_POINT('Ctrl Pts',(149.990291719683,-80.6592985775913,37.2797319931106));
#25026=CARTESIAN_POINT('Ctrl Pts',(149.987499102739,-80.6698565196466,37.2481770331612));
#25027=CARTESIAN_POINT('Ctrl Pts',(149.984157100677,-80.6824881297729,37.2172858271412));
#25028=CARTESIAN_POINT('Ctrl Pts',(149.980355786964,-80.6968505802923,37.1871743733059));
#25029=CARTESIAN_POINT('Ctrl Pts',(149.977558137322,-80.7074209008703,37.1650132720595));
#25030=CARTESIAN_POINT('Ctrl Pts',(149.974509955706,-80.7189351701335,37.1432550493073));
#25031=CARTESIAN_POINT('Ctrl Pts',(149.971243495187,-80.7312708109914,37.1219053194033));
#25032=CARTESIAN_POINT('Ctrl Pts',(149.965898079908,-80.7514575307577,37.0869674495657));
#25033=CARTESIAN_POINT('Ctrl Pts',(149.960009186179,-80.7736866486408,37.0534295032289));
#25034=CARTESIAN_POINT('Ctrl Pts',(149.953740444404,-80.7973352935607,37.0212984264036));
#25035=CARTESIAN_POINT('Ctrl Pts',(149.948225014278,-80.8181420923229,36.9930285254523));
#25036=CARTESIAN_POINT('Ctrl Pts',(149.9424154207,-80.8400482470993,36.9658474797256));
#25037=CARTESIAN_POINT('Ctrl Pts',(149.936415096464,-80.8626613647233,36.9397533647229));
#25038=CARTESIAN_POINT('Ctrl Pts',(149.930229230798,-80.8859737229196,36.9128523700934));
#25039=CARTESIAN_POINT('Ctrl Pts',(149.923781601043,-80.9102578633714,36.8868469814882));
#25040=CARTESIAN_POINT('Ctrl Pts',(149.917129634266,-80.9352949903542,36.8616578829462));
#25041=CARTESIAN_POINT('Ctrl Pts',(149.910169623638,-80.9614915538297,36.8353023103081));
#25042=CARTESIAN_POINT('Ctrl Pts',(149.902985851619,-80.9885126935505,36.8098403335412));
#25043=CARTESIAN_POINT('Ctrl Pts',(149.895629953764,-81.0161619977715,36.7851874043794));
#25044=CARTESIAN_POINT('Ctrl Pts',(149.894768894784,-81.0193985410377,36.7823016076435));
#25045=CARTESIAN_POINT('Ctrl Pts',(149.893905462669,-81.0226437475978,36.7794269040118));
#25046=CARTESIAN_POINT('Ctrl Pts',(149.893039728921,-81.0258973457795,36.7765631636536));
#25047=CARTESIAN_POINT('Ctrl Pts',(149.885294621979,-81.055004985282,36.7509433060931));
#25048=CARTESIAN_POINT('Ctrl Pts',(149.877335285324,-81.0848961910412,36.7261125791076));
#25049=CARTESIAN_POINT('Ctrl Pts',(149.869211724912,-81.1153826082176,36.7020057412078));
#25050=CARTESIAN_POINT('Ctrl Pts',(149.860756318493,-81.1471143901479,36.6769141432401));
#25051=CARTESIAN_POINT('Ctrl Pts',(149.852122887,-81.1794914280943,36.6526066770636));
#25052=CARTESIAN_POINT('Ctrl Pts',(149.843353240441,-81.2123567795935,36.6290138576965));
#25053=CARTESIAN_POINT('Ctrl Pts',(149.834033859779,-81.2472823286659,36.6039420987476));
#25054=CARTESIAN_POINT('Ctrl Pts',(149.824560562659,-81.2827596737919,36.5796772330571));
#25055=CARTESIAN_POINT('Ctrl Pts',(149.814968902639,-81.3186560159925,36.5561425173913));
#25056=CARTESIAN_POINT('Ctrl Pts',(149.814245534137,-81.3213631890216,36.5543676137774));
#25057=CARTESIAN_POINT('Ctrl Pts',(149.813521486337,-81.3240727682653,36.5525968666255));
#25058=CARTESIAN_POINT('Ctrl Pts',(149.81279677161,-81.3267847076918,36.5508302448381));
#25059=CARTESIAN_POINT('Ctrl Pts',(149.802161746897,-81.3665818053887,36.524905469683));
#25060=CARTESIAN_POINT('Ctrl Pts',(149.791378236575,-81.4068954418303,36.4998550500825));
#25061=CARTESIAN_POINT('Ctrl Pts',(149.780505488345,-81.4474999785173,36.4756491236568));
#25062=CARTESIAN_POINT('Ctrl Pts',(149.766212096436,-81.5008789903217,36.4438278411639));
#25063=CARTESIAN_POINT('Ctrl Pts',(149.75173104415,-81.5548874755345,36.4133414348087));
#25064=CARTESIAN_POINT('Ctrl Pts',(149.7370901728,-81.6094178533075,36.383984521067));
#25065=CARTESIAN_POINT('Ctrl Pts',(149.721679195218,-81.6668165155372,36.3530834408842));
#25066=CARTESIAN_POINT('Ctrl Pts',(149.706091100881,-81.7247936014325,36.3234339148145));
#25067=CARTESIAN_POINT('Ctrl Pts',(149.690345642872,-81.7832715016969,36.2948268672563));
#25068=CARTESIAN_POINT('Ctrl Pts',(149.684002656687,-81.8068290579968,36.283302648186));
#25069=CARTESIAN_POINT('Ctrl Pts',(149.67763399788,-81.8304683944409,36.2719479292514));
#25070=CARTESIAN_POINT('Ctrl Pts',(149.671240444102,-81.854186356593,36.2607502650745));
#25071=CARTESIAN_POINT('Ctrl Pts',(149.663115656512,-81.8843266214971,36.2465205196001));
#25072=CARTESIAN_POINT('Ctrl Pts',(149.654955183208,-81.9145791058626,36.2325522508595));
#25073=CARTESIAN_POINT('Ctrl Pts',(149.646761444289,-81.9449339838539,36.2188226892616));
#25074=CARTESIAN_POINT('Ctrl Pts',(149.629599044989,-82.0085145472408,36.1900650951214));
#25075=CARTESIAN_POINT('Ctrl Pts',(149.612256027528,-82.0726719053387,36.1623178493608));
#25076=CARTESIAN_POINT('Ctrl Pts',(149.594776281622,-82.1372383448972,36.1354843276864));
#25077=CARTESIAN_POINT('Ctrl Pts',(149.575926055079,-82.206867046555,36.1065469526683));
#25078=CARTESIAN_POINT('Ctrl Pts',(149.556916727546,-82.2769718987435,36.0786720183343));
#25079=CARTESIAN_POINT('Ctrl Pts',(149.537787182918,-82.3473991049671,36.0517539381005));
#25080=CARTESIAN_POINT('Ctrl Pts',(149.532245072383,-82.3678029028164,36.043955374207));
#25081=CARTESIAN_POINT('Ctrl Pts',(149.526692780135,-82.388234072127,36.0362372267063));
#25082=CARTESIAN_POINT('Ctrl Pts',(149.521131044556,-82.4086895813368,36.0285971804474));
#25083=CARTESIAN_POINT('Ctrl Pts',(149.513307047732,-82.4374654619684,36.0178495106188));
#25084=CARTESIAN_POINT('Ctrl Pts',(149.505462657808,-82.4662967316413,36.0072540693274));
#25085=CARTESIAN_POINT('Ctrl Pts',(149.497602582526,-82.4951656239004,35.9968087539209));
#25086=CARTESIAN_POINT('Ctrl Pts',(149.466886299739,-82.6079819808148,35.9559896459205));
#25087=CARTESIAN_POINT('Ctrl Pts',(149.435949796432,-82.7213062385209,35.9174537341537));
#25088=CARTESIAN_POINT('Ctrl Pts',(149.404819096531,-82.8350358342388,35.8808341283755));
#25089=CARTESIAN_POINT('Ctrl Pts',(149.382928718768,-82.9150078175565,35.8550840807832));
#25090=CARTESIAN_POINT('Ctrl Pts',(149.360942099001,-82.995181007926,35.830282544477));
#25091=CARTESIAN_POINT('Ctrl Pts',(149.338865605393,-83.0755291035976,35.806313699263));
#25092=CARTESIAN_POINT('Ctrl Pts',(149.30257270251,-83.2076182697845,35.766909843424));
#25093=CARTESIAN_POINT('Ctrl Pts',(149.266041574139,-83.3401623692397,35.7297345827405));
#25094=CARTESIAN_POINT('Ctrl Pts',(149.229255373738,-83.4732146574128,35.6944829487653));
#25095=CARTESIAN_POINT('Ctrl Pts',(149.222100057115,-83.4990947765574,35.6876261220257));
#25096=CARTESIAN_POINT('Ctrl Pts',(149.214935059986,-83.5249942184407,35.6808421975289));
#25097=CARTESIAN_POINT('Ctrl Pts',(149.207760216038,-83.5509135089673,35.6741291032872));
#25098=CARTESIAN_POINT('Ctrl Pts',(149.164019348336,-83.7089284102154,35.633203256085));
#25099=CARTESIAN_POINT('Ctrl Pts',(149.119950314816,-83.8675446159542,35.5949411222291));
#25100=CARTESIAN_POINT('Ctrl Pts',(149.075578120339,-84.026655594328,35.5589506769566));
#25101=CARTESIAN_POINT('Ctrl Pts',(149.050851325548,-84.1153215834144,35.5388946854696));
#25102=CARTESIAN_POINT('Ctrl Pts',(149.026030206988,-84.2041418314762,35.5195449132821));
#25103=CARTESIAN_POINT('Ctrl Pts',(149.001117827171,-84.2931021083258,35.5008388586839));
#25104=CARTESIAN_POINT('Ctrl Pts',(148.961812515426,-84.4334584869728,35.4713255278451));
#25105=CARTESIAN_POINT('Ctrl Pts',(148.922228706232,-84.5743409203763,35.4434175359834));
#25106=CARTESIAN_POINT('Ctrl Pts',(148.882458149795,-84.7154243069172,35.41702373575));
#25107=CARTESIAN_POINT('Ctrl Pts',(148.823378480021,-84.9250054803867,35.3778154082434));
#25108=CARTESIAN_POINT('Ctrl Pts',(148.763691428379,-85.1357176965696,35.341819392481));
#25109=CARTESIAN_POINT('Ctrl Pts',(148.703725142329,-85.3463732562435,35.3088731062242));
#25110=CARTESIAN_POINT('Ctrl Pts',(148.683093735234,-85.4188493239612,35.2975379329324));
#25111=CARTESIAN_POINT('Ctrl Pts',(148.662429146922,-85.4913191022936,35.2865639616474));
#25112=CARTESIAN_POINT('Ctrl Pts',(148.64174438629,-85.5637353575988,35.2759451993142));
#25113=CARTESIAN_POINT('Ctrl Pts',(148.565624143843,-85.8302283090543,35.2368679879471));
#25114=CARTESIAN_POINT('Ctrl Pts',(148.489028565031,-86.0967324995911,35.2024345741489));
#25115=CARTESIAN_POINT('Ctrl Pts',(148.411875341988,-86.3635238183438,35.1722187734539));
#25116=CARTESIAN_POINT('Ctrl Pts',(148.365096720961,-86.5252815453833,35.1538986899371));
#25117=CARTESIAN_POINT('Ctrl Pts',(148.318112978006,-86.6871449972432,35.1371301419325));
#25118=CARTESIAN_POINT('Ctrl Pts',(148.270904619886,-86.8491769961467,35.1218271577707));
#25119=CARTESIAN_POINT('Ctrl Pts',(148.24918654488,-86.9237193705385,35.1147870620956));
#25120=CARTESIAN_POINT('Ctrl Pts',(148.227421070419,-86.9982969676292,35.1080522041553));
#25121=CARTESIAN_POINT('Ctrl Pts',(148.205605817643,-87.0729174681581,35.1016219420904));
#25122=CARTESIAN_POINT('Ctrl Pts',(148.101900684429,-87.4276476666717,35.0710538257873));
#25123=CARTESIAN_POINT('Ctrl Pts',(147.997167488692,-87.7829762387848,35.0474026554915));
#25124=CARTESIAN_POINT('Ctrl Pts',(147.891499227194,-88.1385323929298,35.0306489701688));
#25125=CARTESIAN_POINT('Ctrl Pts',(147.785745335362,-88.4943766789275,35.0138817081711));
#25126=CARTESIAN_POINT('Ctrl Pts',(147.679054863976,-88.850448864948,35.0040231183135));
#25127=CARTESIAN_POINT('Ctrl Pts',(147.571529965732,-89.2063722196202,35.0010024709204));
#25128=CARTESIAN_POINT('Ctrl Pts',(147.547727111396,-89.2851631964492,35.0003337883076));
#25129=CARTESIAN_POINT('Ctrl Pts',(147.523883400527,-89.3639468619882,35.));
#25130=CARTESIAN_POINT('Ctrl Pts',(147.5,-89.4427190999916,35.));
#25131=CARTESIAN_POINT('Origin',(152.5,-80.6225774829854,115.));
#25132=CARTESIAN_POINT('Origin',(152.5,-80.6225774829854,37.5));
#25133=CARTESIAN_POINT('Origin',(121.449578014911,-122.5,32.5));
#25134=CARTESIAN_POINT('Origin',(121.449578014911,-122.5,32.5));
#25135=CARTESIAN_POINT('Ctrl Pts',(150.289855072464,-79.4541343310581,37.5));
#25136=CARTESIAN_POINT('Ctrl Pts',(150.,-80.0024038100394,37.5));
#25137=CARTESIAN_POINT('Ctrl Pts',(150.,-80.6225774829855,37.5));
#25138=CARTESIAN_POINT('Ctrl Pts',(150.28985506853,-79.4541343384987,37.2405761439445));
#25139=CARTESIAN_POINT('Ctrl Pts',(149.999999996126,-80.0024038172978,37.3094148175638));
#25140=CARTESIAN_POINT('Ctrl Pts',(150.,-80.6225774905387,37.370288072025));
#25141=CARTESIAN_POINT('Ctrl Pts',(150.270119749701,-79.4914922605508,36.9888304197613));
#25142=CARTESIAN_POINT('Ctrl Pts',(149.980519833119,-80.0389466368966,37.1241843229264));
#25143=CARTESIAN_POINT('Ctrl Pts',(149.989987226484,-80.6604847938369,37.2444152098049));
#25144=CARTESIAN_POINT('Ctrl Pts',(150.196231486305,-79.6310132970258,36.4987912993743));
#25145=CARTESIAN_POINT('Ctrl Pts',(149.907890955038,-80.1748646486434,36.7663952057901));
#25146=CARTESIAN_POINT('Ctrl Pts',(149.952499797667,-80.8020576101747,36.9993956497629));
#25147=CARTESIAN_POINT('Ctrl Pts',(150.143050717941,-79.7313168859281,36.2679996568594));
#25148=CARTESIAN_POINT('Ctrl Pts',(149.855501091412,-80.272795283317,36.5988602080119));
#25149=CARTESIAN_POINT('Ctrl Pts',(149.925518380098,-80.9038362519448,36.8839998280977));
#25150=CARTESIAN_POINT('Ctrl Pts',(150.01502846971,-79.971931353987,35.8382849920617));
#25151=CARTESIAN_POINT('Ctrl Pts',(149.729850869406,-80.506872138187,36.2906206072006));
#25152=CARTESIAN_POINT('Ctrl Pts',(149.860565913637,-81.1479891679691,36.6691424963629));
#25153=CARTESIAN_POINT('Ctrl Pts',(149.939105635844,-80.1142600764838,35.6362636343074));
#25154=CARTESIAN_POINT('Ctrl Pts',(149.655266820466,-80.6454659182015,36.1475015807484));
#25155=CARTESIAN_POINT('Ctrl Pts',(149.8220462428,-81.2924109599909,36.5681318166794));
#25156=CARTESIAN_POINT('Ctrl Pts',(149.775363670977,-80.4199633406152,35.2663619775736));
#25157=CARTESIAN_POINT('Ctrl Pts',(149.494928348598,-80.9422362487713,35.8896065722342));
#25158=CARTESIAN_POINT('Ctrl Pts',(149.738971273161,-81.6026098603007,36.3831809892611));
#25159=CARTESIAN_POINT('Ctrl Pts',(149.686995608736,-80.5843780010491,35.096414733337));
#25160=CARTESIAN_POINT('Ctrl Pts',(149.408398325687,-81.1018541496878,35.7733074247595));
#25161=CARTESIAN_POINT('Ctrl Pts',(149.694137478568,-81.7694423834459,36.2982073663223));
#25162=CARTESIAN_POINT('Ctrl Pts',(149.500255462679,-80.9302925286903,34.7789058669457));
#25163=CARTESIAN_POINT('Ctrl Pts',(149.226078269656,-81.4367533718067,35.5604730905987));
#25164=CARTESIAN_POINT('Ctrl Pts',(149.599394315017,-82.1204438893779,36.1394529338191));
#25165=CARTESIAN_POINT('Ctrl Pts',(149.401347886678,-81.1127763961003,34.630789292851));
#25166=CARTESIAN_POINT('Ctrl Pts',(149.129574349817,-81.6133256610688,35.4636764519996));
#25167=CARTESIAN_POINT('Ctrl Pts',(149.549213266548,-82.3056113431187,36.0653946460504));
#25168=CARTESIAN_POINT('Ctrl Pts',(149.197899201605,-81.4863922312653,34.3564485886759));
#25169=CARTESIAN_POINT('Ctrl Pts',(148.931653199894,-81.9738530462045,35.2892543852115));
#25170=CARTESIAN_POINT('Ctrl Pts',(149.445992976772,-82.684721528767,35.928224294713));
#25171=CARTESIAN_POINT('Ctrl Pts',(149.093462145135,-81.6773447374821,34.2301909539054));
#25172=CARTESIAN_POINT('Ctrl Pts',(148.830186520417,-82.1578926315274,35.2116962088616));
#25173=CARTESIAN_POINT('Ctrl Pts',(149.393006529828,-82.8784821601051,35.8650954766799));
#25174=CARTESIAN_POINT('Ctrl Pts',(148.773324875584,-82.2599185303359,33.8775006940139));
#25175=CARTESIAN_POINT('Ctrl Pts',(148.518202139789,-82.721231742148,35.0014947689296));
#25176=CARTESIAN_POINT('Ctrl Pts',(149.230583943609,-83.4696232145796,35.6887503475526));
#25177=CARTESIAN_POINT('Ctrl Pts',(148.550873607932,-82.6611103319713,33.6767887272455));
#25178=CARTESIAN_POINT('Ctrl Pts',(148.30315471628,-83.1060920248233,34.8943924369605));
#25179=CARTESIAN_POINT('Ctrl Pts',(149.117722639557,-83.8767148956951,35.5883943633349));
#25180=CARTESIAN_POINT('Ctrl Pts',(148.091214058598,-83.4818155626998,33.3265667074903));
#25181=CARTESIAN_POINT('Ctrl Pts',(147.862495369544,-83.8874214153556,34.7305155228013));
#25182=CARTESIAN_POINT('Ctrl Pts',(148.884513014786,-84.7094893209564,35.413283354033));
#25183=CARTESIAN_POINT('Ctrl Pts',(147.853104568995,-83.9028862659541,33.1771134341875));
#25184=CARTESIAN_POINT('Ctrl Pts',(147.635229789714,-84.2865819284461,34.6752930801319));
#25185=CARTESIAN_POINT('Ctrl Pts',(148.763707465283,-85.1367522404598,35.3385567168472));
#25186=CARTESIAN_POINT('Ctrl Pts',(147.37234266623,-84.7444834282146,32.926677827892));
#25187=CARTESIAN_POINT('Ctrl Pts',(147.180928816249,-85.0771956930356,34.6125828689674));
#25188=CARTESIAN_POINT('Ctrl Pts',(148.519791499647,-85.9907258315643,35.2133389141925));
#25189=CARTESIAN_POINT('Ctrl Pts',(147.128665473946,-85.166872640511,32.8248617968328));
#25190=CARTESIAN_POINT('Ctrl Pts',(146.952267516985,-85.4713149459729,34.6060731019583));
#25191=CARTESIAN_POINT('Ctrl Pts',(148.396161159612,-86.4193266499342,35.162430898305));
#25192=CARTESIAN_POINT('Ctrl Pts',(146.388097896077,-86.4377602232181,32.58126559787));
#25193=CARTESIAN_POINT('Ctrl Pts',(146.253862108749,-86.6644852388335,34.6540449090446));
#25194=CARTESIAN_POINT('Ctrl Pts',(148.020432020732,-87.7089037559046,35.0406327991578));
#25195=CARTESIAN_POINT('Ctrl Pts',(145.881711078451,-87.289917999924,32.5000000009063));
#25196=CARTESIAN_POINT('Ctrl Pts',(145.791767290438,-87.4382443129918,34.7842689266371));
#25197=CARTESIAN_POINT('Ctrl Pts',(147.763515165397,-88.573593311031,35.));
#25198=CARTESIAN_POINT('Ctrl Pts',(145.36231884058,-88.1464478086874,32.5));
#25199=CARTESIAN_POINT('Ctrl Pts',(145.36231884058,-88.1464478086874,35.0000000000001));
#25200=CARTESIAN_POINT('Ctrl Pts',(147.5,-89.4427190999917,35.));
#25201=CARTESIAN_POINT('Origin',(147.5,-89.4427190999916,32.5));
#25202=CARTESIAN_POINT('Origin',(0.,0.,32.5));
#25203=CARTESIAN_POINT('',(0.,0.,0.));
#25204=CARTESIAN_POINT('Origin',(0.,0.,137.5));
#25205=CARTESIAN_POINT('',(-37.0000000000001,-4.53119315684522E-15,137.5));
#25206=CARTESIAN_POINT('Origin',(0.,0.,137.5));
#25207=CARTESIAN_POINT('',(-35.,-4.28626379701574E-15,135.5));
#25208=CARTESIAN_POINT('',(-37.0000000000001,-4.53119315684522E-15,137.5));
#25209=CARTESIAN_POINT('',(35.,4.28626379701574E-15,135.5));
#25210=CARTESIAN_POINT('Origin',(0.,0.,135.5));
#25211=CARTESIAN_POINT('Origin',(0.,0.,135.5));
#25212=CARTESIAN_POINT('Origin',(0.,0.,0.999999999999973));
#25213=CARTESIAN_POINT('',(30.,3.67394039744206E-15,0.999999999999973));
#25214=CARTESIAN_POINT('',(-30.,-3.67394039744206E-15,0.999999999999973));
#25215=CARTESIAN_POINT('Origin',(0.,0.,0.999999999999973));
#25216=CARTESIAN_POINT('Origin',(0.,0.,0.999999999999973));
#25217=CARTESIAN_POINT('',(-29.0000000000001,-3.55147571752733E-15,1.38777878078145E-16));
#25218=CARTESIAN_POINT('',(-30.,-3.67394039744206E-15,0.999999999999973));
#25219=CARTESIAN_POINT('Origin',(0.,0.,0.));
#25220=CARTESIAN_POINT('Origin',(0.,0.,88.4999999999999));
#25221=CARTESIAN_POINT('',(35.,4.28626379701574E-15,88.4999999999999));
#25222=CARTESIAN_POINT('',(-35.,-4.28626379701574E-15,88.4999999999999));
#25223=CARTESIAN_POINT('Origin',(0.,0.,88.4999999999999));
#25224=CARTESIAN_POINT('Origin',(0.,0.,88.4999999999999));
#25225=CARTESIAN_POINT('',(-34.0000000000001,-4.16379911710102E-15,87.5));
#25226=CARTESIAN_POINT('',(-35.,-4.28626379701574E-15,88.4999999999999));
#25227=CARTESIAN_POINT('Origin',(0.,0.,87.5));
#25228=CARTESIAN_POINT('Origin',(0.,0.,342.5));
#25229=CARTESIAN_POINT('',(-3.,9.01387818865997,150.));
#25230=CARTESIAN_POINT('',(3.,9.01387818865997,150.));
#25231=CARTESIAN_POINT('Origin',(0.,0.,150.));
#25232=CARTESIAN_POINT('',(3.,9.01387818865997,0.));
#25233=CARTESIAN_POINT('',(3.,9.01387818865997,342.5));
#25234=CARTESIAN_POINT('',(-3.,9.01387818865997,0.));
#25235=CARTESIAN_POINT('Origin',(0.,0.,0.));
#25236=CARTESIAN_POINT('',(-3.,9.01387818865997,342.5));
#25237=CARTESIAN_POINT('Origin',(0.,0.,342.5));
#25238=CARTESIAN_POINT('',(120.,-1.46957615897682E-14,342.5));
#25239=CARTESIAN_POINT('Origin',(0.,0.,342.5));
#25240=CARTESIAN_POINT('',(120.,-1.46957615897682E-14,330.));
#25241=CARTESIAN_POINT('',(120.,-1.46957615897682E-14,342.5));
#25242=CARTESIAN_POINT('',(114.126781955419,-37.0820393249926,330.));
#25243=CARTESIAN_POINT('Origin',(0.,0.,330.));
#25244=CARTESIAN_POINT('',(112.827292588217,-40.8656585314966,330.));
#25245=CARTESIAN_POINT('Origin',(0.,0.,330.));
#25246=CARTESIAN_POINT('',(70.5342302750976,-97.0820393249931,330.));
#25247=CARTESIAN_POINT('Origin',(0.,0.,330.));
#25248=CARTESIAN_POINT('',(67.2589657231482,-99.3792308777461,330.));
#25249=CARTESIAN_POINT('Origin',(0.,0.,330.));
#25250=CARTESIAN_POINT('',(0.,-120.,330.));
#25251=CARTESIAN_POINT('Origin',(0.,0.,330.));
#25252=CARTESIAN_POINT('',(-4.,-119.93331480452,330.));
#25253=CARTESIAN_POINT('Origin',(0.,0.,330.));
#25254=CARTESIAN_POINT('',(-70.5342302750962,-97.0820393249941,330.));
#25255=CARTESIAN_POINT('Origin',(0.,0.,330.));
#25256=CARTESIAN_POINT('',(-73.7311016781464,-94.6769488594074,330.));
#25257=CARTESIAN_POINT('Origin',(0.,0.,330.));
#25258=CARTESIAN_POINT('',(-114.126781955418,-37.0820393249942,330.));
#25259=CARTESIAN_POINT('Origin',(0.,0.,330.));
#25260=CARTESIAN_POINT('',(-115.299428543216,-33.2572064011369,330.));
#25261=CARTESIAN_POINT('Origin',(0.,0.,330.));
#25262=CARTESIAN_POINT('',(-114.126781955419,37.0820393249934,330.));
#25263=CARTESIAN_POINT('Origin',(0.,0.,330.));
#25264=CARTESIAN_POINT('',(-112.827292588217,40.8656585314973,330.));
#25265=CARTESIAN_POINT('Origin',(0.,0.,330.));
#25266=CARTESIAN_POINT('',(-70.5342302750969,97.0820393249936,330.));
#25267=CARTESIAN_POINT('Origin',(0.,0.,330.));
#25268=CARTESIAN_POINT('',(-67.2589657231475,99.3792308777467,330.));
#25269=CARTESIAN_POINT('Origin',(0.,0.,330.));
#25270=CARTESIAN_POINT('',(0.,120.,330.));
#25271=CARTESIAN_POINT('Origin',(0.,0.,330.));
#25272=CARTESIAN_POINT('',(4.,119.93331480452,330.));
#25273=CARTESIAN_POINT('Origin',(0.,0.,330.));
#25274=CARTESIAN_POINT('',(70.5342302750955,97.0820393249946,330.));
#25275=CARTESIAN_POINT('Origin',(0.,0.,330.));
#25276=CARTESIAN_POINT('',(73.7311016781457,94.6769488594079,330.));
#25277=CARTESIAN_POINT('Origin',(0.,0.,330.));
#25278=CARTESIAN_POINT('',(114.126781955418,37.082039324995,330.));
#25279=CARTESIAN_POINT('Origin',(0.,0.,330.));
#25280=CARTESIAN_POINT('',(115.299428543216,33.2572064011377,330.));
#25281=CARTESIAN_POINT('Origin',(0.,0.,330.));
#25282=CARTESIAN_POINT('Origin',(0.,0.,330.));
#25283=CARTESIAN_POINT('Origin',(0.,0.,150.));
#25284=CARTESIAN_POINT('',(160.,-1.95943487863577E-14,137.5));
#25285=CARTESIAN_POINT('Origin',(0.,0.,137.5));
#25286=CARTESIAN_POINT('',(160.,-1.95943487863577E-14,150.));
#25287=CARTESIAN_POINT('',(160.,-1.95943487863577E-14,150.));
#25288=CARTESIAN_POINT('',(152.169042607225,-49.4427190999901,150.));
#25289=CARTESIAN_POINT('Origin',(0.,0.,150.));
#25290=CARTESIAN_POINT('',(152.169042607225,-49.4427190999901,330.));
#25291=CARTESIAN_POINT('',(152.169042607225,-49.4427190999901,330.));
#25292=CARTESIAN_POINT('',(160.,-1.95943487863577E-14,330.));
#25293=CARTESIAN_POINT('Origin',(0.,0.,330.));
#25294=CARTESIAN_POINT('',(160.,-1.95943487863577E-14,342.5));
#25295=CARTESIAN_POINT('',(160.,-1.95943487863577E-14,150.));
#25296=CARTESIAN_POINT('Origin',(0.,0.,342.5));
#25297=CARTESIAN_POINT('',(159.780725560732,8.37375299887273,330.));
#25298=CARTESIAN_POINT('Origin',(0.,0.,330.));
#25299=CARTESIAN_POINT('',(159.780725560732,8.37375299887273,150.));
#25300=CARTESIAN_POINT('',(159.780725560732,8.37375299887273,330.));
#25301=CARTESIAN_POINT('Origin',(0.,0.,150.));
#25302=CARTESIAN_POINT('',(-152.169042607225,49.4427190999912,330.));
#25303=CARTESIAN_POINT('',(-159.780725560732,-8.37375299887161,330.));
#25304=CARTESIAN_POINT('Origin',(0.,0.,330.));
#25305=CARTESIAN_POINT('',(-159.780725560732,-8.37375299887161,150.));
#25306=CARTESIAN_POINT('',(-159.780725560732,-8.37375299887161,330.));
#25307=CARTESIAN_POINT('',(-152.169042607225,49.4427190999912,150.));
#25308=CARTESIAN_POINT('Origin',(0.,0.,150.));
#25309=CARTESIAN_POINT('',(-152.169042607225,49.4427190999912,330.));
#25310=CARTESIAN_POINT('',(94.0456403667969,-129.442719099991,330.));
#25311=CARTESIAN_POINT('',(94.0456403667969,-129.442719099991,150.));
#25312=CARTESIAN_POINT('',(94.0456403667969,-129.442719099991,330.));
#25313=CARTESIAN_POINT('',(134.187290871269,-87.1422456024031,330.));
#25314=CARTESIAN_POINT('Origin',(0.,0.,330.));
#25315=CARTESIAN_POINT('',(134.187290871269,-87.1422456024031,150.));
#25316=CARTESIAN_POINT('',(134.187290871269,-87.1422456024031,330.));
#25317=CARTESIAN_POINT('Origin',(0.,0.,150.));
#25318=CARTESIAN_POINT('',(0.,-160.,330.));
#25319=CARTESIAN_POINT('',(0.,-160.,150.));
#25320=CARTESIAN_POINT('',(0.,-160.,330.));
#25321=CARTESIAN_POINT('',(57.3388719272493,-149.372868239552,330.));
#25322=CARTESIAN_POINT('Origin',(0.,0.,330.));
#25323=CARTESIAN_POINT('',(57.3388719272493,-149.372868239552,150.));
#25324=CARTESIAN_POINT('',(57.3388719272493,-149.372868239552,330.));
#25325=CARTESIAN_POINT('Origin',(0.,0.,150.));
#25326=CARTESIAN_POINT('',(-94.045640366795,-129.442719099992,330.));
#25327=CARTESIAN_POINT('',(-94.045640366795,-129.442719099992,150.));
#25328=CARTESIAN_POINT('',(-94.045640366795,-129.442719099992,330.));
#25329=CARTESIAN_POINT('',(-41.4110472164034,-154.548132206251,330.));
#25330=CARTESIAN_POINT('Origin',(0.,0.,330.));
#25331=CARTESIAN_POINT('',(-41.4110472164034,-154.548132206251,150.));
#25332=CARTESIAN_POINT('',(-41.4110472164034,-154.548132206251,330.));
#25333=CARTESIAN_POINT('Origin',(0.,0.,150.));
#25334=CARTESIAN_POINT('',(-152.169042607224,-49.4427190999923,330.));
#25335=CARTESIAN_POINT('',(-152.169042607224,-49.4427190999923,150.));
#25336=CARTESIAN_POINT('',(-152.169042607224,-49.4427190999923,330.));
#25337=CARTESIAN_POINT('',(-124.343353833115,-100.691262567975,330.));
#25338=CARTESIAN_POINT('Origin',(0.,0.,330.));
#25339=CARTESIAN_POINT('',(-124.343353833115,-100.691262567975,150.));
#25340=CARTESIAN_POINT('',(-124.343353833115,-100.691262567975,330.));
#25341=CARTESIAN_POINT('Origin',(0.,0.,150.));
#25342=CARTESIAN_POINT('',(94.045640366794,129.442719099993,330.));
#25343=CARTESIAN_POINT('',(41.4110472164034,154.548132206251,330.));
#25344=CARTESIAN_POINT('Origin',(0.,0.,330.));
#25345=CARTESIAN_POINT('',(41.4110472164034,154.548132206251,150.));
#25346=CARTESIAN_POINT('',(41.4110472164034,154.548132206251,330.));
#25347=CARTESIAN_POINT('',(94.045640366794,129.442719099993,150.));
#25348=CARTESIAN_POINT('Origin',(0.,0.,150.));
#25349=CARTESIAN_POINT('',(94.045640366794,129.442719099993,330.));
#25350=CARTESIAN_POINT('',(152.169042607224,49.4427190999933,330.));
#25351=CARTESIAN_POINT('',(152.169042607224,49.4427190999933,150.));
#25352=CARTESIAN_POINT('',(152.169042607224,49.4427190999933,330.));
#25353=CARTESIAN_POINT('',(124.343353833114,100.691262567976,330.));
#25354=CARTESIAN_POINT('Origin',(0.,0.,330.));
#25355=CARTESIAN_POINT('',(124.343353833114,100.691262567976,150.));
#25356=CARTESIAN_POINT('',(124.343353833114,100.691262567976,330.));
#25357=CARTESIAN_POINT('Origin',(0.,0.,150.));
#25358=CARTESIAN_POINT('',(-94.0456403667959,129.442719099992,330.));
#25359=CARTESIAN_POINT('',(-94.0456403667959,129.442719099991,150.));
#25360=CARTESIAN_POINT('',(-94.0456403667959,129.442719099992,330.));
#25361=CARTESIAN_POINT('',(-134.187290871268,87.142245602404,330.));
#25362=CARTESIAN_POINT('Origin',(0.,0.,330.));
#25363=CARTESIAN_POINT('',(-134.187290871268,87.142245602404,150.));
#25364=CARTESIAN_POINT('',(-134.187290871268,87.142245602404,330.));
#25365=CARTESIAN_POINT('Origin',(0.,0.,150.));
#25366=CARTESIAN_POINT('',(0.,160.,330.));
#25367=CARTESIAN_POINT('',(0.,160.,150.));
#25368=CARTESIAN_POINT('',(0.,160.,330.));
#25369=CARTESIAN_POINT('',(-57.3388719272482,149.372868239552,330.));
#25370=CARTESIAN_POINT('Origin',(0.,0.,330.));
#25371=CARTESIAN_POINT('',(-57.3388719272482,149.372868239552,150.));
#25372=CARTESIAN_POINT('',(-57.3388719272482,149.372868239552,330.));
#25373=CARTESIAN_POINT('Origin',(0.,0.,150.));
#25374=CARTESIAN_POINT('Origin',(0.,0.,137.5));
#25375=CARTESIAN_POINT('',(35.,-4.28626379701574E-15,137.5));
#25376=CARTESIAN_POINT('Origin',(0.,0.,87.5));
#25377=CARTESIAN_POINT('',(30.,-3.67394039744206E-15,87.5));
#25378=CARTESIAN_POINT('',(30.,-3.67394039744206E-15,87.5));
#25379=CARTESIAN_POINT('Origin',(0.,0.,87.5));
#25380=CARTESIAN_POINT('Origin',(0.,0.,330.));
#25381=CARTESIAN_POINT('',(0.,105.,330.));
#25382=CARTESIAN_POINT('',(0.,95.,330.));
#25383=CARTESIAN_POINT('',(4.,105.,330.));
#25384=CARTESIAN_POINT('',(4.,105.,330.));
#25385=CARTESIAN_POINT('',(4.,95.,330.));
#25386=CARTESIAN_POINT('Origin',(0.,0.,330.));
#25387=CARTESIAN_POINT('',(-61.7174514907098,84.9467844093694,330.));
#25388=CARTESIAN_POINT('',(-55.8395989677851,76.85661446562,330.));
#25389=CARTESIAN_POINT('',(-58.48138351321,87.2979254185393,330.));
#25390=CARTESIAN_POINT('',(-58.48138351321,87.2979254185393,330.));
#25391=CARTESIAN_POINT('',(-52.6035309902853,79.2077554747898,330.));
#25392=CARTESIAN_POINT('Origin',(0.,0.,330.));
#25393=CARTESIAN_POINT('',(-99.8609342109912,32.4467844093692,330.));
#25394=CARTESIAN_POINT('',(-90.3503690480397,29.3566144656198,330.));
#25395=CARTESIAN_POINT('',(-98.6248662334914,36.2510104745498,330.));
#25396=CARTESIAN_POINT('',(-98.6248662334914,36.2510104745498,330.));
#25397=CARTESIAN_POINT('',(-89.1143010705399,33.1608405308004,330.));
#25398=CARTESIAN_POINT('Origin',(0.,0.,330.));
#25399=CARTESIAN_POINT('',(-99.860934210991,-32.4467844093699,330.));
#25400=CARTESIAN_POINT('',(-90.3503690480395,-29.3566144656204,330.));
#25401=CARTESIAN_POINT('',(-101.097002188491,-28.6425583441893,330.));
#25402=CARTESIAN_POINT('',(-101.097002188491,-28.6425583441893,330.));
#25403=CARTESIAN_POINT('',(-91.5864370255393,-25.5523884004398,330.));
#25404=CARTESIAN_POINT('Origin',(0.,0.,330.));
#25405=CARTESIAN_POINT('',(-61.7174514907092,-84.9467844093698,330.));
#25406=CARTESIAN_POINT('',(-55.8395989677845,-76.8566144656203,330.));
#25407=CARTESIAN_POINT('',(-64.953519468209,-82.5956434001999,330.));
#25408=CARTESIAN_POINT('',(-64.953519468209,-82.5956434001999,330.));
#25409=CARTESIAN_POINT('',(-59.0756669452843,-74.5054734564505,330.));
#25410=CARTESIAN_POINT('Origin',(0.,0.,330.));
#25411=CARTESIAN_POINT('',(0.,-105.,330.));
#25412=CARTESIAN_POINT('',(0.,-95.,330.));
#25413=CARTESIAN_POINT('',(-4.,-105.,330.));
#25414=CARTESIAN_POINT('',(-4.,-105.,330.));
#25415=CARTESIAN_POINT('',(-4.,-95.,330.));
#25416=CARTESIAN_POINT('Origin',(0.,0.,330.));
#25417=CARTESIAN_POINT('',(61.7174514907104,-84.9467844093689,330.));
#25418=CARTESIAN_POINT('',(55.8395989677856,-76.8566144656195,330.));
#25419=CARTESIAN_POINT('',(58.4813835132107,-87.2979254185389,330.));
#25420=CARTESIAN_POINT('',(58.4813835132107,-87.2979254185389,330.));
#25421=CARTESIAN_POINT('',(52.6035309902859,-79.2077554747894,330.));
#25422=CARTESIAN_POINT('Origin',(0.,0.,330.));
#25423=CARTESIAN_POINT('',(99.8609342109914,-32.4467844093685,330.));
#25424=CARTESIAN_POINT('',(90.3503690480399,-29.3566144656191,330.));
#25425=CARTESIAN_POINT('',(98.6248662334917,-36.2510104745491,330.));
#25426=CARTESIAN_POINT('',(98.6248662334917,-36.2510104745491,330.));
#25427=CARTESIAN_POINT('',(89.1143010705401,-33.1608405307998,330.));
#25428=CARTESIAN_POINT('Origin',(0.,0.,330.));
#25429=CARTESIAN_POINT('',(99.8609342109908,32.4467844093706,330.));
#25430=CARTESIAN_POINT('',(90.3503690480393,29.356614465621,330.));
#25431=CARTESIAN_POINT('',(101.097002188491,28.64255834419,330.));
#25432=CARTESIAN_POINT('',(101.097002188491,28.64255834419,330.));
#25433=CARTESIAN_POINT('',(91.5864370255391,25.5523884004404,330.));
#25434=CARTESIAN_POINT('Origin',(0.,0.,330.));
#25435=CARTESIAN_POINT('',(61.7174514907085,84.9467844093703,330.));
#25436=CARTESIAN_POINT('',(55.8395989677839,76.8566144656207,330.));
#25437=CARTESIAN_POINT('',(64.9535194682084,82.5956434002004,330.));
#25438=CARTESIAN_POINT('',(64.9535194682084,82.5956434002004,330.));
#25439=CARTESIAN_POINT('',(59.0756669452838,74.5054734564509,330.));
#25440=CARTESIAN_POINT('Origin',(0.,0.,150.));
#25441=CARTESIAN_POINT('',(121.234769987286,98.1739810037762,150.));
#25442=CARTESIAN_POINT('',(124.343353833114,100.691262567976,150.));
#25443=CARTESIAN_POINT('',(94.9004195456003,123.814015240881,150.));
#25444=CARTESIAN_POINT('Origin',(0.,0.,150.));
#25445=CARTESIAN_POINT('',(59.0756669452838,74.5054734564509,150.));
#25446=CARTESIAN_POINT('',(59.0756669452838,74.5054734564509,150.));
#25447=CARTESIAN_POINT('',(55.8395989677839,76.8566144656207,150.));
#25448=CARTESIAN_POINT('',(55.8395989677839,76.8566144656207,150.));
#25449=CARTESIAN_POINT('',(55.8395989677839,76.8566144656207,150.));
#25450=CARTESIAN_POINT('',(40.3757710359933,150.684428901095,150.));
#25451=CARTESIAN_POINT('',(41.4110472164034,154.548132206251,150.));
#25452=CARTESIAN_POINT('',(4.00000000000002,155.948709516943,150.));
#25453=CARTESIAN_POINT('Origin',(0.,0.,150.));
#25454=CARTESIAN_POINT('',(4.,95.,150.));
#25455=CARTESIAN_POINT('',(4.,95.,150.));
#25456=CARTESIAN_POINT('',(0.,95.,150.));
#25457=CARTESIAN_POINT('',(0.,95.,150.));
#25458=CARTESIAN_POINT('',(0.,95.,150.));
#25459=CARTESIAN_POINT('',(-55.905400129067,145.638546533563,150.));
#25460=CARTESIAN_POINT('',(-57.3388719272482,149.372868239552,150.));
#25461=CARTESIAN_POINT('',(-88.4282835906026,128.516297259219,150.));
#25462=CARTESIAN_POINT('Origin',(0.,0.,150.));
#25463=CARTESIAN_POINT('',(-52.6035309902853,79.2077554747898,150.));
#25464=CARTESIAN_POINT('',(-52.6035309902853,79.2077554747898,150.));
#25465=CARTESIAN_POINT('',(-55.8395989677851,76.85661446562,150.));
#25466=CARTESIAN_POINT('',(-55.8395989677851,76.85661446562,150.));
#25467=CARTESIAN_POINT('',(-55.8395989677851,76.85661446562,150.));
#25468=CARTESIAN_POINT('',(-130.832608599486,84.963689462344,150.));
#25469=CARTESIAN_POINT('',(-134.187290871268,87.142245602404,150.));
#25470=CARTESIAN_POINT('',(-147.079968416409,51.9950275567578,150.));
#25471=CARTESIAN_POINT('Origin',(0.,0.,150.));
#25472=CARTESIAN_POINT('',(-89.1143010705399,33.1608405308004,150.));
#25473=CARTESIAN_POINT('',(-89.1143010705399,33.1608405308004,150.));
#25474=CARTESIAN_POINT('',(-90.3503690480397,29.3566144656197,150.));
#25475=CARTESIAN_POINT('',(-90.3503690480397,29.3566144656198,150.));
#25476=CARTESIAN_POINT('',(-90.3503690480397,29.3566144656198,150.));
#25477=CARTESIAN_POINT('',(-155.786207421714,-8.16440917389982,150.));
#25478=CARTESIAN_POINT('',(-159.780725560732,-8.37375299887161,150.));
#25479=CARTESIAN_POINT('',(-149.552104371409,-44.3865754263977,150.));
#25480=CARTESIAN_POINT('Origin',(0.,0.,150.));
#25481=CARTESIAN_POINT('',(-91.5864370255393,-25.5523884004398,150.));
#25482=CARTESIAN_POINT('',(-91.5864370255393,-25.5523884004398,150.));
#25483=CARTESIAN_POINT('',(-90.3503690480395,-29.3566144656204,150.));
#25484=CARTESIAN_POINT('',(-90.3503690480395,-29.3566144656204,150.));
#25485=CARTESIAN_POINT('',(-90.3503690480395,-29.3566144656204,150.));
#25486=CARTESIAN_POINT('',(-121.234769987287,-98.1739810037753,150.));
#25487=CARTESIAN_POINT('',(-124.343353833115,-100.691262567975,150.));
#25488=CARTESIAN_POINT('',(-94.9004195456013,-123.81401524088,150.));
#25489=CARTESIAN_POINT('Origin',(0.,0.,150.));
#25490=CARTESIAN_POINT('',(-59.0756669452843,-74.5054734564505,150.));
#25491=CARTESIAN_POINT('',(-59.0756669452843,-74.5054734564505,150.));
#25492=CARTESIAN_POINT('',(-55.8395989677845,-76.8566144656203,150.));
#25493=CARTESIAN_POINT('',(-55.8395989677845,-76.8566144656203,150.));
#25494=CARTESIAN_POINT('',(-55.8395989677845,-76.8566144656203,150.));
#25495=CARTESIAN_POINT('',(-40.3757710359933,-150.684428901095,150.));
#25496=CARTESIAN_POINT('',(-41.4110472164034,-154.548132206251,150.));
#25497=CARTESIAN_POINT('',(-4.,-155.948709516943,150.));
#25498=CARTESIAN_POINT('Origin',(0.,0.,150.));
#25499=CARTESIAN_POINT('',(-4.,-95.,150.));
#25500=CARTESIAN_POINT('',(-4.,-95.,150.));
#25501=CARTESIAN_POINT('',(0.,-95.,150.));
#25502=CARTESIAN_POINT('',(0.,-95.,150.));
#25503=CARTESIAN_POINT('',(0.,-95.,150.));
#25504=CARTESIAN_POINT('',(55.905400129068,-145.638546533563,150.));
#25505=CARTESIAN_POINT('',(57.3388719272493,-149.372868239552,150.));
#25506=CARTESIAN_POINT('',(88.4282835906036,-128.516297259218,150.));
#25507=CARTESIAN_POINT('Origin',(0.,0.,150.));
#25508=CARTESIAN_POINT('',(52.6035309902859,-79.2077554747895,150.));
#25509=CARTESIAN_POINT('',(52.6035309902859,-79.2077554747894,150.));
#25510=CARTESIAN_POINT('',(55.8395989677856,-76.8566144656195,150.));
#25511=CARTESIAN_POINT('',(55.8395989677856,-76.8566144656195,150.));
#25512=CARTESIAN_POINT('',(55.8395989677856,-76.8566144656195,150.));
#25513=CARTESIAN_POINT('',(130.832608599487,-84.9636894623431,150.));
#25514=CARTESIAN_POINT('',(134.187290871269,-87.1422456024031,150.));
#25515=CARTESIAN_POINT('',(147.07996841641,-51.9950275567568,150.));
#25516=CARTESIAN_POINT('Origin',(0.,0.,150.));
#25517=CARTESIAN_POINT('',(89.1143010705401,-33.1608405307998,150.));
#25518=CARTESIAN_POINT('',(89.1143010705401,-33.1608405307998,150.));
#25519=CARTESIAN_POINT('',(90.3503690480399,-29.3566144656191,150.));
#25520=CARTESIAN_POINT('',(90.3503690480399,-29.3566144656191,150.));
#25521=CARTESIAN_POINT('',(90.3503690480399,-29.3566144656191,150.));
#25522=CARTESIAN_POINT('',(155.786207421713,8.16440917390091,150.));
#25523=CARTESIAN_POINT('',(159.780725560732,8.37375299887273,150.));
#25524=CARTESIAN_POINT('',(149.552104371408,44.3865754263987,150.));
#25525=CARTESIAN_POINT('Origin',(0.,0.,150.));
#25526=CARTESIAN_POINT('',(91.5864370255391,25.5523884004404,150.));
#25527=CARTESIAN_POINT('',(91.5864370255391,25.5523884004404,150.));
#25528=CARTESIAN_POINT('',(90.3503690480393,29.356614465621,150.));
#25529=CARTESIAN_POINT('',(90.3503690480393,29.356614465621,150.));
#25530=CARTESIAN_POINT('',(90.3503690480393,29.356614465621,150.));
#25531=CARTESIAN_POINT('',(3.,12.3,150.));
#25532=CARTESIAN_POINT('',(3.,-7.91840766518671E-16,150.));
#25533=CARTESIAN_POINT('',(-3.,12.3,150.));
#25534=CARTESIAN_POINT('',(-3.,-7.91840766518671E-16,150.));
#25535=CARTESIAN_POINT('',(0.,12.3,150.));
#25536=CARTESIAN_POINT('Origin',(0.,0.,0.));
#25537=CARTESIAN_POINT('',(3.,12.3,0.));
#25538=CARTESIAN_POINT('',(3.,12.3,0.));
#25539=CARTESIAN_POINT('',(-3.,12.3,0.));
#25540=CARTESIAN_POINT('',(3.,12.3,0.));
#25541=CARTESIAN_POINT('',(-3.,12.3,0.));
#25542=CARTESIAN_POINT('Origin',(0.,0.,87.5));
#25543=CARTESIAN_POINT('Origin',(0.,0.,137.5));
#25544=CARTESIAN_POINT('Origin',(0.,95.,330.));
#25545=CARTESIAN_POINT('',(4.,95.,320.));
#25546=CARTESIAN_POINT('',(4.,95.,330.));
#25547=CARTESIAN_POINT('',(0.,95.,320.));
#25548=CARTESIAN_POINT('',(0.,95.,320.));
#25549=CARTESIAN_POINT('',(0.,95.,330.));
#25550=CARTESIAN_POINT('Origin',(4.,95.,330.));
#25551=CARTESIAN_POINT('Origin',(4.,105.,320.));
#25552=CARTESIAN_POINT('',(4.00000000000002,155.948709516943,330.));
#25553=CARTESIAN_POINT('',(4.00000000000002,155.948709516943,330.));
#25554=CARTESIAN_POINT('',(4.,95.,330.));
#25555=CARTESIAN_POINT('Origin',(0.,0.,330.));
#25556=CARTESIAN_POINT('',(40.3757710359933,150.684428901095,330.));
#25557=CARTESIAN_POINT('',(40.3757710359933,150.684428901095,330.));
#25558=CARTESIAN_POINT('Origin',(0.,0.,330.));
#25559=CARTESIAN_POINT('Origin',(41.4110472164034,154.548132206251,330.));
#25560=CARTESIAN_POINT('',(41.4110472164034,154.548132206251,330.));
#25561=CARTESIAN_POINT('Origin',(0.,95.,330.));
#25562=CARTESIAN_POINT('Origin',(0.,105.,320.));
#25563=CARTESIAN_POINT('',(0.,95.,330.));
#25564=CARTESIAN_POINT('Origin',(0.,105.,320.));
#25565=CARTESIAN_POINT('Origin',(-55.8395989677851,76.85661446562,330.));
#25566=CARTESIAN_POINT('',(-52.6035309902853,79.2077554747898,320.));
#25567=CARTESIAN_POINT('',(-52.6035309902853,79.2077554747898,330.));
#25568=CARTESIAN_POINT('',(-55.8395989677851,76.85661446562,320.));
#25569=CARTESIAN_POINT('',(-55.8395989677851,76.85661446562,320.));
#25570=CARTESIAN_POINT('',(-55.8395989677851,76.85661446562,330.));
#25571=CARTESIAN_POINT('Origin',(-52.6035309902853,79.2077554747898,330.));
#25572=CARTESIAN_POINT('Origin',(-58.48138351321,87.2979254185393,320.));
#25573=CARTESIAN_POINT('',(-88.4282835906026,128.516297259219,330.));
#25574=CARTESIAN_POINT('',(-88.4282835906026,128.516297259219,330.));
#25575=CARTESIAN_POINT('',(-52.6035309902853,79.2077554747898,330.));
#25576=CARTESIAN_POINT('Origin',(0.,0.,330.));
#25577=CARTESIAN_POINT('',(-55.905400129067,145.638546533563,330.));
#25578=CARTESIAN_POINT('',(-55.905400129067,145.638546533563,330.));
#25579=CARTESIAN_POINT('Origin',(0.,0.,330.));
#25580=CARTESIAN_POINT('Origin',(-57.3388719272482,149.372868239552,330.));
#25581=CARTESIAN_POINT('',(-57.3388719272482,149.372868239552,330.));
#25582=CARTESIAN_POINT('Origin',(-55.8395989677851,76.85661446562,330.));
#25583=CARTESIAN_POINT('Origin',(-61.7174514907098,84.9467844093694,320.));
#25584=CARTESIAN_POINT('',(-55.8395989677851,76.85661446562,330.));
#25585=CARTESIAN_POINT('Origin',(-90.3503690480397,29.3566144656198,330.));
#25586=CARTESIAN_POINT('',(-89.1143010705399,33.1608405308004,320.));
#25587=CARTESIAN_POINT('',(-89.1143010705399,33.1608405308004,330.));
#25588=CARTESIAN_POINT('',(-90.3503690480397,29.3566144656198,320.));
#25589=CARTESIAN_POINT('',(-90.3503690480397,29.3566144656198,320.));
#25590=CARTESIAN_POINT('',(-90.3503690480397,29.3566144656198,330.));
#25591=CARTESIAN_POINT('Origin',(-89.1143010705399,33.1608405308004,330.));
#25592=CARTESIAN_POINT('Origin',(-98.6248662334914,36.2510104745498,320.));
#25593=CARTESIAN_POINT('',(-147.079968416409,51.9950275567578,330.));
#25594=CARTESIAN_POINT('',(-147.079968416409,51.9950275567578,330.));
#25595=CARTESIAN_POINT('',(-89.1143010705399,33.1608405308004,330.));
#25596=CARTESIAN_POINT('Origin',(0.,0.,330.));
#25597=CARTESIAN_POINT('',(-130.832608599486,84.963689462344,330.));
#25598=CARTESIAN_POINT('',(-130.832608599486,84.963689462344,330.));
#25599=CARTESIAN_POINT('Origin',(0.,0.,330.));
#25600=CARTESIAN_POINT('Origin',(-134.187290871268,87.142245602404,330.));
#25601=CARTESIAN_POINT('',(-134.187290871268,87.142245602404,330.));
#25602=CARTESIAN_POINT('Origin',(-90.3503690480397,29.3566144656198,330.));
#25603=CARTESIAN_POINT('Origin',(-99.8609342109912,32.4467844093692,320.));
#25604=CARTESIAN_POINT('',(-90.3503690480397,29.3566144656198,330.));
#25605=CARTESIAN_POINT('Origin',(-90.3503690480395,-29.3566144656204,330.));
#25606=CARTESIAN_POINT('',(-91.5864370255393,-25.5523884004398,320.));
#25607=CARTESIAN_POINT('',(-91.5864370255393,-25.5523884004398,330.));
#25608=CARTESIAN_POINT('',(-90.3503690480395,-29.3566144656204,320.));
#25609=CARTESIAN_POINT('',(-90.3503690480395,-29.3566144656204,320.));
#25610=CARTESIAN_POINT('',(-90.3503690480395,-29.3566144656204,330.));
#25611=CARTESIAN_POINT('Origin',(-91.5864370255393,-25.5523884004398,330.));
#25612=CARTESIAN_POINT('Origin',(-101.097002188491,-28.6425583441893,320.));
#25613=CARTESIAN_POINT('',(-149.552104371409,-44.3865754263977,330.));
#25614=CARTESIAN_POINT('',(-149.552104371409,-44.3865754263977,330.));
#25615=CARTESIAN_POINT('',(-91.5864370255393,-25.5523884004398,330.));
#25616=CARTESIAN_POINT('Origin',(0.,0.,330.));
#25617=CARTESIAN_POINT('',(-155.786207421714,-8.16440917389982,330.));
#25618=CARTESIAN_POINT('',(-155.786207421714,-8.16440917389982,330.));
#25619=CARTESIAN_POINT('Origin',(0.,0.,330.));
#25620=CARTESIAN_POINT('Origin',(-159.780725560732,-8.37375299887161,330.));
#25621=CARTESIAN_POINT('',(-159.780725560732,-8.37375299887161,330.));
#25622=CARTESIAN_POINT('Origin',(-90.3503690480395,-29.3566144656204,330.));
#25623=CARTESIAN_POINT('Origin',(-99.860934210991,-32.4467844093699,320.));
#25624=CARTESIAN_POINT('',(-90.3503690480395,-29.3566144656204,330.));
#25625=CARTESIAN_POINT('Origin',(-55.8395989677845,-76.8566144656203,330.));
#25626=CARTESIAN_POINT('',(-59.0756669452843,-74.5054734564505,320.));
#25627=CARTESIAN_POINT('',(-59.0756669452843,-74.5054734564505,330.));
#25628=CARTESIAN_POINT('',(-55.8395989677845,-76.8566144656203,320.));
#25629=CARTESIAN_POINT('',(-55.8395989677845,-76.8566144656203,320.));
#25630=CARTESIAN_POINT('',(-55.8395989677845,-76.8566144656203,330.));
#25631=CARTESIAN_POINT('Origin',(-59.0756669452843,-74.5054734564505,330.));
#25632=CARTESIAN_POINT('Origin',(-64.953519468209,-82.5956434001999,320.));
#25633=CARTESIAN_POINT('',(-94.9004195456013,-123.81401524088,330.));
#25634=CARTESIAN_POINT('',(-94.9004195456013,-123.81401524088,330.));
#25635=CARTESIAN_POINT('',(-59.0756669452843,-74.5054734564505,330.));
#25636=CARTESIAN_POINT('Origin',(0.,0.,330.));
#25637=CARTESIAN_POINT('',(-121.234769987287,-98.1739810037753,330.));
#25638=CARTESIAN_POINT('',(-121.234769987287,-98.1739810037753,330.));
#25639=CARTESIAN_POINT('Origin',(0.,0.,330.));
#25640=CARTESIAN_POINT('Origin',(-124.343353833115,-100.691262567975,330.));
#25641=CARTESIAN_POINT('',(-124.343353833115,-100.691262567975,330.));
#25642=CARTESIAN_POINT('Origin',(-55.8395989677845,-76.8566144656203,330.));
#25643=CARTESIAN_POINT('Origin',(-61.7174514907092,-84.9467844093698,320.));
#25644=CARTESIAN_POINT('',(-55.8395989677845,-76.8566144656203,330.));
#25645=CARTESIAN_POINT('Origin',(0.,-95.,330.));
#25646=CARTESIAN_POINT('',(-4.,-95.,320.));
#25647=CARTESIAN_POINT('',(-4.,-95.,330.));
#25648=CARTESIAN_POINT('',(0.,-95.,320.));
#25649=CARTESIAN_POINT('',(0.,-95.,320.));
#25650=CARTESIAN_POINT('',(0.,-95.,330.));
#25651=CARTESIAN_POINT('Origin',(-4.,-95.,330.));
#25652=CARTESIAN_POINT('Origin',(-4.,-105.,320.));
#25653=CARTESIAN_POINT('',(-4.00000000000002,-155.948709516943,330.));
#25654=CARTESIAN_POINT('',(-4.00000000000002,-155.948709516943,330.));
#25655=CARTESIAN_POINT('',(-4.,-95.,330.));
#25656=CARTESIAN_POINT('Origin',(0.,0.,330.));
#25657=CARTESIAN_POINT('',(-40.3757710359933,-150.684428901095,330.));
#25658=CARTESIAN_POINT('',(-40.3757710359933,-150.684428901095,330.));
#25659=CARTESIAN_POINT('Origin',(0.,0.,330.));
#25660=CARTESIAN_POINT('Origin',(-41.4110472164034,-154.548132206251,330.));
#25661=CARTESIAN_POINT('',(-41.4110472164034,-154.548132206251,330.));
#25662=CARTESIAN_POINT('Origin',(0.,-95.,330.));
#25663=CARTESIAN_POINT('Origin',(0.,-105.,320.));
#25664=CARTESIAN_POINT('',(0.,-95.,330.));
#25665=CARTESIAN_POINT('Origin',(55.8395989677856,-76.8566144656195,330.));
#25666=CARTESIAN_POINT('',(52.6035309902859,-79.2077554747894,320.));
#25667=CARTESIAN_POINT('',(52.6035309902859,-79.2077554747894,330.));
#25668=CARTESIAN_POINT('',(55.8395989677856,-76.8566144656195,320.));
#25669=CARTESIAN_POINT('',(55.8395989677856,-76.8566144656195,320.));
#25670=CARTESIAN_POINT('',(55.8395989677856,-76.8566144656195,330.));
#25671=CARTESIAN_POINT('Origin',(52.6035309902859,-79.2077554747894,330.));
#25672=CARTESIAN_POINT('Origin',(58.4813835132107,-87.2979254185389,320.));
#25673=CARTESIAN_POINT('',(88.4282835906035,-128.516297259218,330.));
#25674=CARTESIAN_POINT('',(88.4282835906035,-128.516297259218,330.));
#25675=CARTESIAN_POINT('',(52.6035309902859,-79.2077554747894,330.));
#25676=CARTESIAN_POINT('Origin',(0.,0.,330.));
#25677=CARTESIAN_POINT('',(55.905400129068,-145.638546533563,330.));
#25678=CARTESIAN_POINT('',(55.905400129068,-145.638546533563,330.));
#25679=CARTESIAN_POINT('Origin',(0.,0.,330.));
#25680=CARTESIAN_POINT('Origin',(57.3388719272493,-149.372868239552,330.));
#25681=CARTESIAN_POINT('',(57.3388719272493,-149.372868239552,330.));
#25682=CARTESIAN_POINT('Origin',(55.8395989677856,-76.8566144656195,330.));
#25683=CARTESIAN_POINT('Origin',(61.7174514907104,-84.9467844093689,320.));
#25684=CARTESIAN_POINT('',(55.8395989677856,-76.8566144656195,330.));
#25685=CARTESIAN_POINT('Origin',(90.3503690480399,-29.3566144656191,330.));
#25686=CARTESIAN_POINT('',(89.1143010705401,-33.1608405307998,320.));
#25687=CARTESIAN_POINT('',(89.1143010705401,-33.1608405307998,330.));
#25688=CARTESIAN_POINT('',(90.3503690480399,-29.3566144656191,320.));
#25689=CARTESIAN_POINT('',(90.3503690480399,-29.3566144656191,320.));
#25690=CARTESIAN_POINT('',(90.3503690480399,-29.3566144656191,330.));
#25691=CARTESIAN_POINT('Origin',(89.1143010705401,-33.1608405307998,330.));
#25692=CARTESIAN_POINT('Origin',(98.6248662334917,-36.2510104745491,320.));
#25693=CARTESIAN_POINT('',(147.07996841641,-51.9950275567568,330.));
#25694=CARTESIAN_POINT('',(147.07996841641,-51.9950275567568,330.));
#25695=CARTESIAN_POINT('',(89.1143010705401,-33.1608405307998,330.));
#25696=CARTESIAN_POINT('Origin',(0.,0.,330.));
#25697=CARTESIAN_POINT('',(130.832608599487,-84.9636894623431,330.));
#25698=CARTESIAN_POINT('',(130.832608599487,-84.9636894623431,330.));
#25699=CARTESIAN_POINT('Origin',(0.,0.,330.));
#25700=CARTESIAN_POINT('Origin',(134.187290871269,-87.1422456024031,330.));
#25701=CARTESIAN_POINT('',(134.187290871269,-87.1422456024031,330.));
#25702=CARTESIAN_POINT('Origin',(90.3503690480399,-29.3566144656191,330.));
#25703=CARTESIAN_POINT('Origin',(99.8609342109914,-32.4467844093685,320.));
#25704=CARTESIAN_POINT('',(90.3503690480399,-29.3566144656191,330.));
#25705=CARTESIAN_POINT('Origin',(90.3503690480393,29.356614465621,330.));
#25706=CARTESIAN_POINT('',(91.5864370255391,25.5523884004404,320.));
#25707=CARTESIAN_POINT('',(91.5864370255391,25.5523884004404,330.));
#25708=CARTESIAN_POINT('',(90.3503690480393,29.356614465621,320.));
#25709=CARTESIAN_POINT('',(90.3503690480393,29.356614465621,320.));
#25710=CARTESIAN_POINT('',(90.3503690480393,29.356614465621,330.));
#25711=CARTESIAN_POINT('Origin',(91.5864370255391,25.5523884004404,330.));
#25712=CARTESIAN_POINT('Origin',(101.097002188491,28.64255834419,320.));
#25713=CARTESIAN_POINT('',(149.552104371408,44.3865754263987,330.));
#25714=CARTESIAN_POINT('',(149.552104371408,44.3865754263987,330.));
#25715=CARTESIAN_POINT('',(91.5864370255391,25.5523884004404,330.));
#25716=CARTESIAN_POINT('Origin',(0.,0.,330.));
#25717=CARTESIAN_POINT('',(155.786207421713,8.16440917390091,330.));
#25718=CARTESIAN_POINT('',(155.786207421713,8.16440917390091,330.));
#25719=CARTESIAN_POINT('Origin',(0.,0.,330.));
#25720=CARTESIAN_POINT('Origin',(159.780725560732,8.37375299887273,330.));
#25721=CARTESIAN_POINT('',(159.780725560732,8.37375299887273,330.));
#25722=CARTESIAN_POINT('Origin',(90.3503690480393,29.356614465621,330.));
#25723=CARTESIAN_POINT('Origin',(99.8609342109908,32.4467844093706,320.));
#25724=CARTESIAN_POINT('',(90.3503690480393,29.356614465621,330.));
#25725=CARTESIAN_POINT('Origin',(55.8395989677839,76.8566144656207,330.));
#25726=CARTESIAN_POINT('',(59.0756669452838,74.5054734564509,320.));
#25727=CARTESIAN_POINT('',(59.0756669452838,74.5054734564509,330.));
#25728=CARTESIAN_POINT('',(55.8395989677839,76.8566144656207,320.));
#25729=CARTESIAN_POINT('',(55.8395989677839,76.8566144656207,320.));
#25730=CARTESIAN_POINT('',(55.8395989677839,76.8566144656207,330.));
#25731=CARTESIAN_POINT('Origin',(59.0756669452838,74.5054734564509,330.));
#25732=CARTESIAN_POINT('Origin',(64.9535194682084,82.5956434002004,320.));
#25733=CARTESIAN_POINT('',(94.9004195456004,123.814015240881,330.));
#25734=CARTESIAN_POINT('',(94.9004195456004,123.814015240881,330.));
#25735=CARTESIAN_POINT('',(59.0756669452838,74.5054734564509,330.));
#25736=CARTESIAN_POINT('Origin',(0.,0.,330.));
#25737=CARTESIAN_POINT('',(121.234769987286,98.1739810037762,330.));
#25738=CARTESIAN_POINT('',(121.234769987286,98.1739810037762,330.));
#25739=CARTESIAN_POINT('Origin',(0.,0.,330.));
#25740=CARTESIAN_POINT('Origin',(124.343353833114,100.691262567976,330.));
#25741=CARTESIAN_POINT('',(124.343353833114,100.691262567976,330.));
#25742=CARTESIAN_POINT('Origin',(55.8395989677839,76.8566144656207,330.));
#25743=CARTESIAN_POINT('Origin',(61.7174514907085,84.9467844093703,320.));
#25744=CARTESIAN_POINT('',(55.8395989677839,76.8566144656207,330.));
#25745=CARTESIAN_POINT('Origin',(-61.7174514907098,84.9467844093694,320.));
#25746=CARTESIAN_POINT('Origin',(-99.8609342109912,32.4467844093692,320.));
#25747=CARTESIAN_POINT('Origin',(-99.860934210991,-32.4467844093699,320.));
#25748=CARTESIAN_POINT('Origin',(-61.7174514907092,-84.9467844093698,320.));
#25749=CARTESIAN_POINT('Origin',(0.,-105.,320.));
#25750=CARTESIAN_POINT('Origin',(61.7174514907104,-84.9467844093689,320.));
#25751=CARTESIAN_POINT('Origin',(99.8609342109914,-32.4467844093685,320.));
#25752=CARTESIAN_POINT('Origin',(99.8609342109908,32.4467844093706,320.));
#25753=CARTESIAN_POINT('Origin',(61.7174514907085,84.9467844093703,320.));
#25754=CARTESIAN_POINT('Origin',(0.,0.,330.));
#25755=CARTESIAN_POINT('Origin',(0.,0.,330.));
#25756=CARTESIAN_POINT('Origin',(0.,0.,330.));
#25757=CARTESIAN_POINT('Origin',(0.,0.,330.));
#25758=CARTESIAN_POINT('Origin',(0.,0.,330.));
#25759=CARTESIAN_POINT('Origin',(0.,0.,330.));
#25760=CARTESIAN_POINT('Origin',(0.,0.,330.));
#25761=CARTESIAN_POINT('Origin',(0.,0.,330.));
#25762=CARTESIAN_POINT('Origin',(0.,0.,330.));
#25763=CARTESIAN_POINT('Origin',(0.,0.,330.));
#25764=CARTESIAN_POINT('Origin',(0.,0.,342.5));
#25765=CARTESIAN_POINT('Origin',(3.,12.3,342.5));
#25766=CARTESIAN_POINT('',(3.,12.3,342.5));
#25767=CARTESIAN_POINT('Origin',(3.,12.3,342.5));
#25768=CARTESIAN_POINT('',(-3.,12.3,342.5));
#25769=CARTESIAN_POINT('Origin',(-3.,12.3,342.5));
#25770=CARTESIAN_POINT('',(0.,0.,0.));
#25771=CARTESIAN_POINT('Origin',(0.,0.,11.5));
#25772=CARTESIAN_POINT('',(-194.,-2.37581479034587E-14,12.5));
#25773=CARTESIAN_POINT('Origin',(0.,0.,12.5));
#25774=CARTESIAN_POINT('',(-195.,-2.38806125833734E-14,11.5));
#25775=CARTESIAN_POINT('Origin',(-194.,-2.37581479034587E-14,11.5));
#25776=CARTESIAN_POINT('',(195.,2.38806125833734E-14,11.5));
#25777=CARTESIAN_POINT('Origin',(0.,0.,11.5));
#25778=CARTESIAN_POINT('Origin',(0.,0.,11.5));
#25779=CARTESIAN_POINT('Origin',(0.,0.,1.));
#25780=CARTESIAN_POINT('',(195.,2.38806125833734E-14,1.));
#25781=CARTESIAN_POINT('',(-195.,-2.38806125833734E-14,1.));
#25782=CARTESIAN_POINT('Origin',(0.,0.,1.));
#25783=CARTESIAN_POINT('Origin',(0.,0.,1.));
#25784=CARTESIAN_POINT('',(-194.,-2.37581479034587E-14,0.));
#25785=CARTESIAN_POINT('Origin',(-194.,-2.37581479034587E-14,1.));
#25786=CARTESIAN_POINT('Origin',(0.,0.,0.));
#25787=CARTESIAN_POINT('Origin',(155.884572681198,90.0000000000018,12.5));
#25788=CARTESIAN_POINT('',(150.384572681198,90.0000000000018,12.));
#25789=CARTESIAN_POINT('Origin',(155.884572681198,90.0000000000018,12.));
#25790=CARTESIAN_POINT('',(149.884572681198,90.0000000000018,12.5));
#25791=CARTESIAN_POINT('',(149.884572681198,90.0000000000018,12.5));
#25792=CARTESIAN_POINT('Origin',(155.884572681198,90.0000000000018,12.5));
#25793=CARTESIAN_POINT('Origin',(155.884572681198,90.0000000000018,12.5));
#25794=CARTESIAN_POINT('',(150.384572681198,90.0000000000018,0.));
#25795=CARTESIAN_POINT('Origin',(155.884572681198,90.0000000000018,0.));
#25796=CARTESIAN_POINT('',(150.384572681198,90.0000000000018,12.5));
#25797=CARTESIAN_POINT('Origin',(155.8845726812,-89.9999999999986,12.5));
#25798=CARTESIAN_POINT('',(150.3845726812,-89.9999999999986,12.));
#25799=CARTESIAN_POINT('Origin',(155.8845726812,-89.9999999999986,12.));
#25800=CARTESIAN_POINT('',(149.8845726812,-89.9999999999986,12.5));
#25801=CARTESIAN_POINT('',(149.8845726812,-89.9999999999986,12.5));
#25802=CARTESIAN_POINT('Origin',(155.8845726812,-89.9999999999986,12.5));
#25803=CARTESIAN_POINT('Origin',(155.8845726812,-89.9999999999986,12.5));
#25804=CARTESIAN_POINT('',(150.3845726812,-89.9999999999986,0.));
#25805=CARTESIAN_POINT('Origin',(155.8845726812,-89.9999999999986,0.));
#25806=CARTESIAN_POINT('',(150.3845726812,-89.9999999999986,12.5));
#25807=CARTESIAN_POINT('Origin',(0.,-180.,12.5));
#25808=CARTESIAN_POINT('',(-5.5,-180.,12.));
#25809=CARTESIAN_POINT('Origin',(0.,-180.,12.));
#25810=CARTESIAN_POINT('',(-6.,-180.,12.5));
#25811=CARTESIAN_POINT('',(-6.,-180.,12.5));
#25812=CARTESIAN_POINT('Origin',(0.,-180.,12.5));
#25813=CARTESIAN_POINT('Origin',(0.,-180.,12.5));
#25814=CARTESIAN_POINT('',(-5.49999999999999,-180.,0.));
#25815=CARTESIAN_POINT('Origin',(0.,-180.,0.));
#25816=CARTESIAN_POINT('',(-5.49999999999999,-180.,12.5));
#25817=CARTESIAN_POINT('Origin',(-155.884572681199,-90.0000000000007,12.5));
#25818=CARTESIAN_POINT('',(-161.384572681199,-90.0000000000007,12.));
#25819=CARTESIAN_POINT('Origin',(-155.884572681199,-90.0000000000007,12.));
#25820=CARTESIAN_POINT('',(-161.884572681199,-90.0000000000007,12.5));
#25821=CARTESIAN_POINT('',(-161.884572681199,-90.0000000000007,12.5));
#25822=CARTESIAN_POINT('Origin',(-155.884572681199,-90.0000000000007,12.5));
#25823=CARTESIAN_POINT('Origin',(-155.884572681199,-90.0000000000007,12.5));
#25824=CARTESIAN_POINT('',(-161.384572681199,-90.0000000000007,0.));
#25825=CARTESIAN_POINT('Origin',(-155.884572681199,-90.0000000000007,0.));
#25826=CARTESIAN_POINT('',(-161.384572681199,-90.0000000000007,12.5));
#25827=CARTESIAN_POINT('Origin',(-155.884572681199,89.9999999999996,12.5));
#25828=CARTESIAN_POINT('',(-161.384572681199,89.9999999999996,12.));
#25829=CARTESIAN_POINT('Origin',(-155.884572681199,89.9999999999996,12.));
#25830=CARTESIAN_POINT('',(-161.884572681199,89.9999999999996,12.5));
#25831=CARTESIAN_POINT('',(-161.884572681199,89.9999999999996,12.5));
#25832=CARTESIAN_POINT('Origin',(-155.884572681199,89.9999999999996,12.5));
#25833=CARTESIAN_POINT('Origin',(-155.884572681199,89.9999999999996,12.5));
#25834=CARTESIAN_POINT('',(-161.384572681199,89.9999999999996,0.));
#25835=CARTESIAN_POINT('Origin',(-155.884572681199,89.9999999999996,0.));
#25836=CARTESIAN_POINT('',(-161.384572681199,89.9999999999996,12.5));
#25837=CARTESIAN_POINT('Origin',(0.,180.,12.5));
#25838=CARTESIAN_POINT('',(-5.5,180.,12.));
#25839=CARTESIAN_POINT('Origin',(0.,180.,12.));
#25840=CARTESIAN_POINT('',(-6.,180.,12.5));
#25841=CARTESIAN_POINT('',(-6.,180.,12.5));
#25842=CARTESIAN_POINT('Origin',(0.,180.,12.5));
#25843=CARTESIAN_POINT('Origin',(0.,180.,12.5));
#25844=CARTESIAN_POINT('',(-5.49999999999999,180.,0.));
#25845=CARTESIAN_POINT('Origin',(0.,180.,0.));
#25846=CARTESIAN_POINT('',(-5.49999999999999,180.,12.5));
#25847=CARTESIAN_POINT('Origin',(0.,0.,12.5));
#25848=CARTESIAN_POINT('',(145.,-1.77573785876366E-14,12.5));
#25849=CARTESIAN_POINT('Origin',(0.,0.,12.5));
#25850=CARTESIAN_POINT('',(145.,-1.77573785876366E-14,0.));
#25851=CARTESIAN_POINT('',(145.,-1.77573785876366E-14,12.5));
#25852=CARTESIAN_POINT('Origin',(0.,0.,0.));
#25853=CARTESIAN_POINT('Origin',(0.,0.,12.5));
#25854=CARTESIAN_POINT('',(195.,-2.38806125833734E-14,12.5));
#25855=CARTESIAN_POINT('Origin',(0.,0.,12.5));
#25856=CARTESIAN_POINT('Origin',(0.,0.,0.));
#25857=CARTESIAN_POINT('',(0.,0.,0.));
#25858=CARTESIAN_POINT('Origin',(38.0492,-76.2,-180.));
#25859=CARTESIAN_POINT('',(0.,-76.2,180.));
#25860=CARTESIAN_POINT('',(38.0492,-76.2,180.));
#25861=CARTESIAN_POINT('',(38.0492,-76.2,180.));
#25862=CARTESIAN_POINT('',(0.,-76.2,-180.));
#25863=CARTESIAN_POINT('',(0.,-76.2,-180.));
#25864=CARTESIAN_POINT('',(38.0492,-76.2,-180.));
#25865=CARTESIAN_POINT('',(38.0492,-76.2,-180.));
#25866=CARTESIAN_POINT('',(38.0492,-76.2,-180.));
#25867=CARTESIAN_POINT('Origin',(0.,-76.2,-180.));
#25868=CARTESIAN_POINT('',(0.,-74.042335135838,180.));
#25869=CARTESIAN_POINT('',(0.,-76.2,180.));
#25870=CARTESIAN_POINT('',(0.,-74.042335135838,-180.));
#25871=CARTESIAN_POINT('',(0.,-74.042335135838,-180.));
#25872=CARTESIAN_POINT('',(0.,-76.2,-180.));
#25873=CARTESIAN_POINT('Origin',(2.54,-74.042335135838,-180.));
#25874=CARTESIAN_POINT('',(2.12239693365934,-71.5368995092487,180.));
#25875=CARTESIAN_POINT('Origin',(2.54,-74.042335135838,180.));
#25876=CARTESIAN_POINT('',(2.12239693365934,-71.5368995092487,-180.));
#25877=CARTESIAN_POINT('',(2.12239693365934,-71.5368995092487,-180.));
#25878=CARTESIAN_POINT('Origin',(2.54,-74.042335135838,-180.));
#25879=CARTESIAN_POINT('Origin',(25.7655282791198,-67.5960901573836,-180.));
#25880=CARTESIAN_POINT('',(25.7655282791198,-67.5960901573836,180.));
#25881=CARTESIAN_POINT('',(25.7655282791198,-67.5960901573836,180.));
#25882=CARTESIAN_POINT('',(25.7655282791198,-67.5960901573836,-180.));
#25883=CARTESIAN_POINT('',(25.7655282791198,-67.5960901573836,-180.));
#25884=CARTESIAN_POINT('',(25.7655282791198,-67.5960901573836,-180.));
#25885=CARTESIAN_POINT('Origin',(24.638,-60.8314139655925,-180.));
#25886=CARTESIAN_POINT('',(31.496,-60.8314139655925,180.));
#25887=CARTESIAN_POINT('Origin',(24.638,-60.8314139655925,180.));
#25888=CARTESIAN_POINT('',(31.496,-60.8314139655925,-180.));
#25889=CARTESIAN_POINT('',(31.496,-60.8314139655925,-180.));
#25890=CARTESIAN_POINT('Origin',(24.638,-60.8314139655925,-180.));
#25891=CARTESIAN_POINT('Origin',(31.496,-15.3685860344075,-180.));
#25892=CARTESIAN_POINT('',(31.496,-15.3685860344075,180.));
#25893=CARTESIAN_POINT('',(31.496,-15.3685860344075,180.));
#25894=CARTESIAN_POINT('',(31.496,-15.3685860344075,-180.));
#25895=CARTESIAN_POINT('',(31.496,-15.3685860344075,-180.));
#25896=CARTESIAN_POINT('',(31.496,-15.3685860344075,-180.));
#25897=CARTESIAN_POINT('Origin',(24.638,-15.3685860344075,-180.));
#25898=CARTESIAN_POINT('',(25.7655282791198,-8.60390984261643,180.));
#25899=CARTESIAN_POINT('Origin',(24.638,-15.3685860344075,180.));
#25900=CARTESIAN_POINT('',(25.7655282791198,-8.60390984261643,-180.));
#25901=CARTESIAN_POINT('',(25.7655282791198,-8.60390984261643,-180.));
#25902=CARTESIAN_POINT('Origin',(24.638,-15.3685860344075,-180.));
#25903=CARTESIAN_POINT('Origin',(25.7655282791198,-8.60390984261643,-180.));
#25904=CARTESIAN_POINT('',(2.12239693365934,-4.66310049075127,180.));
#25905=CARTESIAN_POINT('',(25.7655282791198,-8.60390984261642,180.));
#25906=CARTESIAN_POINT('',(2.12239693365934,-4.66310049075127,-180.));
#25907=CARTESIAN_POINT('',(2.12239693365934,-4.66310049075127,-180.));
#25908=CARTESIAN_POINT('',(25.7655282791198,-8.60390984261643,-180.));
#25909=CARTESIAN_POINT('Origin',(2.54,-2.15766486416198,-180.));
#25910=CARTESIAN_POINT('',(0.,-2.15766486416198,180.));
#25911=CARTESIAN_POINT('Origin',(2.54,-2.15766486416198,180.));
#25912=CARTESIAN_POINT('',(0.,-2.15766486416198,-180.));
#25913=CARTESIAN_POINT('',(0.,-2.15766486416198,-180.));
#25914=CARTESIAN_POINT('Origin',(2.54,-2.15766486416198,-180.));
#25915=CARTESIAN_POINT('Origin',(0.,0.,-180.));
#25916=CARTESIAN_POINT('',(0.,0.,180.));
#25917=CARTESIAN_POINT('',(0.,0.,180.));
#25918=CARTESIAN_POINT('',(0.,0.,-180.));
#25919=CARTESIAN_POINT('',(0.,0.,-180.));
#25920=CARTESIAN_POINT('',(0.,0.,-180.));
#25921=CARTESIAN_POINT('Origin',(38.0492,0.,-180.));
#25922=CARTESIAN_POINT('',(38.0492,0.,180.));
#25923=CARTESIAN_POINT('',(38.0492,0.,180.));
#25924=CARTESIAN_POINT('',(38.0492,0.,-180.));
#25925=CARTESIAN_POINT('',(38.0492,0.,-180.));
#25926=CARTESIAN_POINT('',(38.0492,0.,-180.));
#25927=CARTESIAN_POINT('Origin',(38.0492,-76.2,-180.));
#25928=CARTESIAN_POINT('',(38.0492,-76.2,180.));
#25929=CARTESIAN_POINT('',(38.0492,-76.2,-180.));
#25930=CARTESIAN_POINT('Origin',(0.,-76.2,-180.));
#25931=CARTESIAN_POINT('Origin',(-3.46944695195361E-15,0.,180.));
#25932=CARTESIAN_POINT('Origin',(38.0491999999999,-76.2,-180.));
#25933=CARTESIAN_POINT('',(38.0491999999999,-76.2,180.));
#25934=CARTESIAN_POINT('',(38.0491999999999,-74.042335135838,180.));
#25935=CARTESIAN_POINT('',(38.0491999999999,-76.2,180.));
#25936=CARTESIAN_POINT('',(38.0491999999999,-71.5368995092488,177.877603066341));
#25937=CARTESIAN_POINT('Origin',(38.0491999999999,-74.042335135838,177.46));
#25938=CARTESIAN_POINT('',(38.0491999999999,-67.5960901573836,154.23447172088));
#25939=CARTESIAN_POINT('',(38.0491999999999,-67.5960901573836,154.23447172088));
#25940=CARTESIAN_POINT('',(38.0491999999999,-60.8314139655925,148.504));
#25941=CARTESIAN_POINT('Origin',(38.0491999999999,-60.8314139655925,155.362));
#25942=CARTESIAN_POINT('',(38.0491999999999,-15.3685860344075,148.504));
#25943=CARTESIAN_POINT('',(38.0491999999999,-15.3685860344075,148.504));
#25944=CARTESIAN_POINT('',(38.0491999999999,-8.6039098426164,154.23447172088));
#25945=CARTESIAN_POINT('Origin',(38.0491999999999,-15.3685860344075,155.362));
#25946=CARTESIAN_POINT('',(38.0491999999999,-4.66310049075123,177.877603066341));
#25947=CARTESIAN_POINT('',(38.0491999999999,-8.6039098426164,154.23447172088));
#25948=CARTESIAN_POINT('',(38.0491999999999,-2.15766486416195,180.));
#25949=CARTESIAN_POINT('Origin',(38.0491999999999,-2.15766486416195,177.46));
#25950=CARTESIAN_POINT('',(38.0491999999999,3.46944695195361E-14,180.));
#25951=CARTESIAN_POINT('',(38.0491999999999,3.46944695195361E-14,180.));
#25952=CARTESIAN_POINT('',(38.0491999999999,2.08166817117217E-14,141.9508));
#25953=CARTESIAN_POINT('',(38.0491999999999,2.08166817117217E-14,-180.));
#25954=CARTESIAN_POINT('',(38.0491999999999,-76.2,141.9508));
#25955=CARTESIAN_POINT('',(38.0491999999999,-76.2,141.9508));
#25956=CARTESIAN_POINT('',(38.0491999999999,-76.2,-180.));
#25957=CARTESIAN_POINT('Origin',(-1.38777878078145E-13,-76.2,141.9508));
#25958=CARTESIAN_POINT('',(332.282278663992,1.38777878078145E-14,141.9508));
#25959=CARTESIAN_POINT('',(-8.32667268468867E-14,3.46944695195361E-14,141.9508));
#25960=CARTESIAN_POINT('',(332.282278663992,-76.2,141.9508));
#25961=CARTESIAN_POINT('',(332.282278663992,-76.2,141.9508));
#25962=CARTESIAN_POINT('',(-1.38777878078145E-13,-76.2,141.9508));
#25963=CARTESIAN_POINT('Origin',(-8.32667268468867E-14,3.46944695195361E-14,
141.9508));
#25964=CARTESIAN_POINT('',(340.,3.46944695195361E-14,180.));
#25965=CARTESIAN_POINT('',(-1.11022302462516E-13,4.16333634234434E-14,180.));
#25966=CARTESIAN_POINT('',(319.151687711983,2.77555756156289E-14,77.2155679930824));
#25967=CARTESIAN_POINT('Origin',(-1.11022302462516E-13,4.16333634234434E-14,
180.));
#25968=CARTESIAN_POINT('',(340.,-2.15766486416195,180.));
#25969=CARTESIAN_POINT('',(-1.38777878078145E-13,-2.15766486416193,180.));
#25970=CARTESIAN_POINT('',(340.,3.46944695195361E-14,180.));
#25971=CARTESIAN_POINT('Origin',(-1.66533453693773E-13,-2.15766486416194,
177.46));
#25972=CARTESIAN_POINT('',(339.569502956741,-4.66310049075124,177.877603066341));
#25973=CARTESIAN_POINT('',(-1.66533453693773E-13,-4.66310049075123,177.877603066341));
#25974=CARTESIAN_POINT('Origin',(339.484798308677,-2.15766486416141,177.459999999999));
#25975=CARTESIAN_POINT('Origin',(-1.66533453693773E-13,-8.6039098426164,
154.23447172088));
#25976=CARTESIAN_POINT('',(334.773841044403,-8.60390984261639,154.23447172088));
#25977=CARTESIAN_POINT('',(-1.66533453693773E-13,-8.6039098426164,154.23447172088));
#25978=CARTESIAN_POINT('',(321.888621689571,-19.1922694606555,90.7089481977025));
#25979=CARTESIAN_POINT('Origin',(-1.11022302462516E-13,-15.3685860344075,
155.362));
#25980=CARTESIAN_POINT('',(333.611499027604,-15.3685860344075,148.504));
#25981=CARTESIAN_POINT('',(-1.11022302462516E-13,-15.3685860344075,148.504));
#25982=CARTESIAN_POINT('Origin',(335.002543594174,-15.3685860344077,155.362));
#25983=CARTESIAN_POINT('Origin',(-1.11022302462516E-13,-15.3685860344075,
148.504));
#25984=CARTESIAN_POINT('',(333.611499027604,-60.8314139655925,148.504));
#25985=CARTESIAN_POINT('',(-2.77555756156289E-14,-60.8314139655925,148.504));
#25986=CARTESIAN_POINT('',(333.611499027604,-15.3685860344075,148.504));
#25987=CARTESIAN_POINT('Origin',(-1.38777878078145E-13,-60.8314139655925,
155.362));
#25988=CARTESIAN_POINT('',(334.773841044404,-67.5960901573836,154.23447172088));
#25989=CARTESIAN_POINT('',(-1.94289029309402E-13,-67.5960901573836,154.23447172088));
#25990=CARTESIAN_POINT('Origin',(335.002543594174,-60.8314139655902,155.362000000003));
#25991=CARTESIAN_POINT('Origin',(-1.94289029309402E-13,-67.5960901573836,
154.23447172088));
#25992=CARTESIAN_POINT('',(339.569502956741,-71.5368995092488,177.877603066341));
#25993=CARTESIAN_POINT('',(-1.66533453693773E-13,-71.5368995092487,177.877603066341));
#25994=CARTESIAN_POINT('',(321.888621689571,-57.0077305393445,90.7089481977025));
#25995=CARTESIAN_POINT('Origin',(-8.32667268468867E-14,-74.042335135838,
177.46));
#25996=CARTESIAN_POINT('',(340.,-74.042335135838,180.));
#25997=CARTESIAN_POINT('',(-8.32667268468867E-14,-74.042335135838,180.));
#25998=CARTESIAN_POINT('Origin',(339.484798308678,-74.0423351358383,177.46));
#25999=CARTESIAN_POINT('Origin',(-1.38777878078145E-13,-76.2,180.));
#26000=CARTESIAN_POINT('',(340.,-76.2,180.));
#26001=CARTESIAN_POINT('',(-1.38777878078145E-13,-76.2,180.));
#26002=CARTESIAN_POINT('',(340.,-76.2,180.));
#26003=CARTESIAN_POINT('Origin',(-1.38777878078145E-13,-76.2,141.9508));
#26004=CARTESIAN_POINT('',(319.151687711983,-76.2,77.2155679930824));
#26005=CARTESIAN_POINT('Origin',(334.54009041727,-38.0999999999999,153.08205587497));
#26006=CARTESIAN_POINT('Origin',(334.54009041727,-38.0999999999999,153.08205587497));
#26007=CARTESIAN_POINT('',(340.,-2.15766486416197,180.));
#26008=CARTESIAN_POINT('',(340.,-2.77555756156289E-14,180.));
#26009=CARTESIAN_POINT('',(340.,-3.67761376907083E-13,180.));
#26010=CARTESIAN_POINT('',(332.282278663992,2.42861286636753E-13,141.9508));
#26011=CARTESIAN_POINT('',(327.009283962862,4.16333634234434E-13,115.954366435321));
#26012=CARTESIAN_POINT('',(332.282278663992,-76.1999999999997,141.9508));
#26013=CARTESIAN_POINT('',(332.282278663992,4.85722573273506E-14,141.9508));
#26014=CARTESIAN_POINT('',(340.,-76.2,180.));
#26015=CARTESIAN_POINT('',(327.009283962862,-76.1999999999995,115.954366435321));
#26016=CARTESIAN_POINT('',(340.,-74.042335135838,180.));
#26017=CARTESIAN_POINT('',(340.,-76.2,180.));
#26018=CARTESIAN_POINT('',(339.56950295674,-71.5368995092487,177.87760306634));
#26019=CARTESIAN_POINT('Origin',(339.484798308677,-74.0423351358391,177.459999999999));
#26020=CARTESIAN_POINT('',(334.773841044403,-67.5960901573834,154.23447172088));
#26021=CARTESIAN_POINT('',(329.541995367165,-63.2968491455564,128.44090728968));
#26022=CARTESIAN_POINT('',(333.611499027603,-60.8314139655923,148.504));
#26023=CARTESIAN_POINT('Origin',(335.002543594174,-60.831413965591,155.362000000001));
#26024=CARTESIAN_POINT('',(333.611499027603,-15.3685860344073,148.504));
#26025=CARTESIAN_POINT('',(333.611499027603,-60.8314139655925,148.504));
#26026=CARTESIAN_POINT('',(334.773841044403,-8.60390984261626,154.23447172088));
#26027=CARTESIAN_POINT('Origin',(335.002543594174,-15.3685860344086,155.362000000001));
#26028=CARTESIAN_POINT('',(339.56950295674,-4.66310049075126,177.877603066341));
#26029=CARTESIAN_POINT('',(329.541995367166,-12.9031508544429,128.44090728968));
#26030=CARTESIAN_POINT('Origin',(339.484798308676,-2.1576648641567,177.459999999994));
#26031=CARTESIAN_POINT('Origin',(455.174510060656,2.4980018054066E-13,89.9579328706422));
#26032=CARTESIAN_POINT('',(462.282278663992,2.56739074444567E-13,86.9508));
#26033=CARTESIAN_POINT('',(455.174510060656,2.4980018054066E-13,89.9579328706422));
#26034=CARTESIAN_POINT('',(462.282278663992,-76.1999999999997,86.9507999999995));
#26035=CARTESIAN_POINT('',(462.282278663992,2.70616862252382E-13,86.9508));
#26036=CARTESIAN_POINT('',(455.174510060656,-76.1999999999997,89.9579328706417));
#26037=CARTESIAN_POINT('Origin',(455.174510060656,-76.1999999999997,89.9579328706417));
#26038=CARTESIAN_POINT('',(470.,-76.2,125.));
#26039=CARTESIAN_POINT('',(462.587255030328,-76.1999999999997,88.4543664353206));
#26040=CARTESIAN_POINT('',(470.,-76.2,125.));
#26041=CARTESIAN_POINT('Origin',(470.,-76.2,125.));
#26042=CARTESIAN_POINT('',(470.,-74.042335135838,125.));
#26043=CARTESIAN_POINT('',(470.,-76.2,125.));
#26044=CARTESIAN_POINT('',(470.,-74.042335135838,125.));
#26045=CARTESIAN_POINT('Origin',(469.010314423275,-74.042335135838,122.660743182285));
#26046=CARTESIAN_POINT('',(469.569502956741,-71.5368995092487,122.87760306634));
#26047=CARTESIAN_POINT('Origin',(469.484798308677,-74.0423351358414,122.459999999996));
#26048=CARTESIAN_POINT('',(469.173029278217,-71.5368995092487,123.045341930331));
#26049=CARTESIAN_POINT('Origin',(459.960719797421,-67.5960901573834,101.270792248449));
#26050=CARTESIAN_POINT('',(464.773841044404,-67.5960901573834,99.2344717208798));
#26051=CARTESIAN_POINT('',(464.974992377841,-67.7613851824375,100.226169526879));
#26052=CARTESIAN_POINT('',(459.960719797421,-67.5960901573834,101.270792248449));
#26053=CARTESIAN_POINT('Origin',(460.400049905765,-60.8314139655923,102.309208868173));
#26054=CARTESIAN_POINT('',(463.611499027604,-60.8314139655922,93.5039999999996));
#26055=CARTESIAN_POINT('Origin',(465.002543594174,-60.8314139655914,100.362000000001));
#26056=CARTESIAN_POINT('',(457.727898848607,-60.8314139655922,95.9932154603443));
#26057=CARTESIAN_POINT('Origin',(457.727898848607,-60.8314139655922,95.9932154603443));
#26058=CARTESIAN_POINT('',(463.611499027604,-15.3685860344073,93.5039999999999));
#26059=CARTESIAN_POINT('',(463.611499027604,-60.8314139655922,93.5039999999996));
#26060=CARTESIAN_POINT('',(457.727898848607,-15.3685860344073,95.9932154603446));
#26061=CARTESIAN_POINT('Origin',(460.400049905766,-15.3685860344074,102.309208868173));
#26062=CARTESIAN_POINT('',(464.773841044404,-8.60390984261627,99.2344717208802));
#26063=CARTESIAN_POINT('Origin',(465.002543594175,-15.3685860344111,100.362000000004));
#26064=CARTESIAN_POINT('',(459.960719797421,-8.60390984261627,101.27079224845));
#26065=CARTESIAN_POINT('Origin',(459.960719797421,-8.60390984261625,101.27079224845));
#26066=CARTESIAN_POINT('',(469.569502956741,-4.66310049075126,122.877603066341));
#26067=CARTESIAN_POINT('',(464.974992377841,-8.43861481756216,100.226169526879));
#26068=CARTESIAN_POINT('',(469.173029278217,-4.66310049075127,123.045341930331));
#26069=CARTESIAN_POINT('Origin',(469.010314423275,-2.15766486416197,122.660743182286));
#26070=CARTESIAN_POINT('',(470.,-2.15766486416197,125.));
#26071=CARTESIAN_POINT('Origin',(469.484798308679,-2.15766486416684,122.460000000005));
#26072=CARTESIAN_POINT('',(470.,-2.15766486416197,125.));
#26073=CARTESIAN_POINT('Origin',(470.,6.93889390390723E-15,125.));
#26074=CARTESIAN_POINT('',(470.,6.93889390390723E-15,125.));
#26075=CARTESIAN_POINT('',(470.,6.93889390390723E-15,125.));
#26076=CARTESIAN_POINT('',(470.,6.93889390390723E-15,125.));
#26077=CARTESIAN_POINT('Origin',(455.174510060656,2.4980018054066E-13,89.9579328706422));
#26078=CARTESIAN_POINT('',(462.587255030328,2.35922392732846E-13,88.4543664353211));
#26079=CARTESIAN_POINT('Origin',(464.54009041727,-38.0999999999998,98.0820558749701));
#26080=CARTESIAN_POINT('Origin',(720.,2.70616862252382E-13,86.9508));
#26081=CARTESIAN_POINT('',(681.9508,1.38777878078145E-14,125.));
#26082=CARTESIAN_POINT('',(681.9508,1.38777878078145E-14,86.9507999999998));
#26083=CARTESIAN_POINT('',(681.9508,1.38777878078145E-14,125.));
#26084=CARTESIAN_POINT('',(462.282278663992,2.70616862252382E-13,86.9508));
#26085=CARTESIAN_POINT('',(720.,2.70616862252382E-13,86.9508));
#26086=CARTESIAN_POINT('',(470.,1.38777878078145E-14,125.));
#26087=CARTESIAN_POINT('',(472.466348646758,-6.93889390390723E-14,137.159365289908));
#26088=CARTESIAN_POINT('',(720.,1.38777878078145E-14,125.));
#26089=CARTESIAN_POINT('Origin',(720.,1.38777878078145E-14,125.));
#26090=CARTESIAN_POINT('',(681.9508,-2.15766486416195,125.));
#26091=CARTESIAN_POINT('',(681.9508,1.38777878078145E-14,125.));
#26092=CARTESIAN_POINT('',(470.,-2.15766486416195,125.));
#26093=CARTESIAN_POINT('',(470.,6.17561557447743E-13,125.));
#26094=CARTESIAN_POINT('',(720.,-2.15766486416194,125.));
#26095=CARTESIAN_POINT('Origin',(720.,-2.15766486416195,122.46));
#26096=CARTESIAN_POINT('',(681.9508,-4.66310049075124,122.877603066341));
#26097=CARTESIAN_POINT('Origin',(681.9508,-2.15766486416194,122.46));
#26098=CARTESIAN_POINT('',(469.569502956741,-4.66310049075123,122.877603066341));
#26099=CARTESIAN_POINT('Origin',(469.484798308678,-2.15766486416211,122.46));
#26100=CARTESIAN_POINT('',(720.,-4.66310049075125,122.877603066341));
#26101=CARTESIAN_POINT('Origin',(720.,-8.60390984261621,99.2344717208803));
#26102=CARTESIAN_POINT('',(681.9508,-8.60390984261625,99.2344717208803));
#26103=CARTESIAN_POINT('',(681.9508,-8.60390984261622,99.2344717208803));
#26104=CARTESIAN_POINT('',(464.773841044404,-8.60390984261625,99.2344717208803));
#26105=CARTESIAN_POINT('',(474.597323766275,-0.531515815288028,147.665302857156));
#26106=CARTESIAN_POINT('',(720.,-8.60390984261624,99.2344717208803));
#26107=CARTESIAN_POINT('Origin',(720.,-15.3685860344074,100.362));
#26108=CARTESIAN_POINT('',(681.9508,-15.3685860344073,93.504));
#26109=CARTESIAN_POINT('Origin',(681.9508,-15.3685860344074,100.362));
#26110=CARTESIAN_POINT('',(463.611499027604,-15.3685860344073,93.504));
#26111=CARTESIAN_POINT('Origin',(465.002543594174,-15.368586034407,100.362));
#26112=CARTESIAN_POINT('',(720.,-15.3685860344073,93.504));
#26113=CARTESIAN_POINT('Origin',(720.,-60.8314139655922,93.5039999999996));
#26114=CARTESIAN_POINT('',(681.9508,-60.8314139655923,93.5039999999997));
#26115=CARTESIAN_POINT('',(681.9508,-60.8314139655923,93.5039999999996));
#26116=CARTESIAN_POINT('',(463.611499027604,-60.8314139655923,93.5039999999996));
#26117=CARTESIAN_POINT('',(463.611499027604,-60.8314139655919,93.5039999999996));
#26118=CARTESIAN_POINT('',(720.,-60.8314139655922,93.5039999999996));
#26119=CARTESIAN_POINT('Origin',(720.,-60.8314139655923,100.362));
#26120=CARTESIAN_POINT('',(681.9508,-67.5960901573835,99.2344717208798));
#26121=CARTESIAN_POINT('Origin',(681.9508,-60.8314139655923,100.362));
#26122=CARTESIAN_POINT('',(464.773841044404,-67.5960901573835,99.2344717208798));
#26123=CARTESIAN_POINT('Origin',(465.002543594175,-60.8314139655898,100.362000000003));
#26124=CARTESIAN_POINT('',(720.,-67.5960901573835,99.2344717208798));
#26125=CARTESIAN_POINT('Origin',(720.,-67.5960901573835,99.2344717208798));
#26126=CARTESIAN_POINT('',(681.9508,-71.5368995092487,122.87760306634));
#26127=CARTESIAN_POINT('',(681.9508,-67.5960901573835,99.2344717208798));
#26128=CARTESIAN_POINT('',(469.569502956741,-71.5368995092487,122.87760306634));
#26129=CARTESIAN_POINT('',(474.597323766275,-75.6684841847123,147.665302857156));
#26130=CARTESIAN_POINT('',(720.,-71.5368995092487,122.87760306634));
#26131=CARTESIAN_POINT('Origin',(720.,-74.0423351358381,122.46));
#26132=CARTESIAN_POINT('',(681.9508,-74.042335135838,125.));
#26133=CARTESIAN_POINT('Origin',(681.9508,-74.042335135838,122.46));
#26134=CARTESIAN_POINT('',(470.,-74.042335135838,125.));
#26135=CARTESIAN_POINT('Origin',(469.484798308678,-74.042335135835,122.460000000003));
#26136=CARTESIAN_POINT('',(720.,-74.042335135838,125.));
#26137=CARTESIAN_POINT('Origin',(720.,-76.2,125.));
#26138=CARTESIAN_POINT('',(681.9508,-76.2,125.));
#26139=CARTESIAN_POINT('',(681.9508,-76.2,125.));
#26140=CARTESIAN_POINT('',(470.,-76.2,125.));
#26141=CARTESIAN_POINT('',(470.,-76.2,125.));
#26142=CARTESIAN_POINT('',(720.,-76.2,125.));
#26143=CARTESIAN_POINT('Origin',(720.,-76.1999999999998,86.9507999999995));
#26144=CARTESIAN_POINT('',(681.9508,-76.1999999999997,86.9507999999995));
#26145=CARTESIAN_POINT('',(681.9508,-76.2,125.));
#26146=CARTESIAN_POINT('',(462.282278663992,-76.1999999999997,86.9507999999995));
#26147=CARTESIAN_POINT('',(472.466348646758,-76.2000000000001,137.159365289908));
#26148=CARTESIAN_POINT('',(720.,-76.1999999999998,86.9507999999995));
#26149=CARTESIAN_POINT('Origin',(720.,2.70616862252382E-13,86.9508));
#26150=CARTESIAN_POINT('',(681.9508,2.77555756156289E-13,86.9508));
#26151=CARTESIAN_POINT('',(462.282278663992,6.45317133063372E-13,86.9508));
#26152=CARTESIAN_POINT('Origin',(464.54009041727,-38.0999999999998,98.0820558749701));
#26153=CARTESIAN_POINT('Origin',(681.9508,-76.2,125.));
#26154=CARTESIAN_POINT('Origin',(681.9508,-76.2,125.));
#26155=CARTESIAN_POINT('',(720.,-76.2,-125.));
#26156=CARTESIAN_POINT('',(681.9508,-76.2,-125.));
#26157=CARTESIAN_POINT('',(681.9508,-76.2,-125.));
#26158=CARTESIAN_POINT('',(720.,-76.2,125.));
#26159=CARTESIAN_POINT('',(720.,-76.2,125.));
#26160=CARTESIAN_POINT('',(681.9508,-76.2,125.));
#26161=CARTESIAN_POINT('',(681.9508,-76.2,125.));
#26162=CARTESIAN_POINT('',(681.9508,-76.2,125.));
#26163=CARTESIAN_POINT('Origin',(720.,-76.2,125.));
#26164=CARTESIAN_POINT('',(720.,-74.042335135838,-125.));
#26165=CARTESIAN_POINT('',(720.,-76.2,-125.));
#26166=CARTESIAN_POINT('',(720.,-74.042335135838,125.));
#26167=CARTESIAN_POINT('',(720.,-74.042335135838,125.));
#26168=CARTESIAN_POINT('',(720.,-76.2,125.));
#26169=CARTESIAN_POINT('Origin',(717.46,-74.042335135838,125.));
#26170=CARTESIAN_POINT('',(717.877603066341,-71.5368995092487,-125.));
#26171=CARTESIAN_POINT('Origin',(717.46,-74.042335135838,-125.));
#26172=CARTESIAN_POINT('',(717.877603066341,-71.5368995092487,125.));
#26173=CARTESIAN_POINT('',(717.877603066341,-71.5368995092487,125.));
#26174=CARTESIAN_POINT('Origin',(717.46,-74.042335135838,125.));
#26175=CARTESIAN_POINT('Origin',(694.23447172088,-67.5960901573836,125.));
#26176=CARTESIAN_POINT('',(694.23447172088,-67.5960901573835,-125.));
#26177=CARTESIAN_POINT('',(694.23447172088,-67.5960901573836,-125.));
#26178=CARTESIAN_POINT('',(694.23447172088,-67.5960901573835,125.));
#26179=CARTESIAN_POINT('',(694.23447172088,-67.5960901573835,125.));
#26180=CARTESIAN_POINT('',(694.23447172088,-67.5960901573836,125.));
#26181=CARTESIAN_POINT('Origin',(695.362,-60.8314139655925,125.));
#26182=CARTESIAN_POINT('',(688.504,-60.8314139655925,-125.));
#26183=CARTESIAN_POINT('Origin',(695.362,-60.8314139655925,-125.));
#26184=CARTESIAN_POINT('',(688.504,-60.8314139655925,125.));
#26185=CARTESIAN_POINT('',(688.504,-60.8314139655925,125.));
#26186=CARTESIAN_POINT('Origin',(695.362,-60.8314139655925,125.));
#26187=CARTESIAN_POINT('Origin',(688.504,-15.3685860344075,125.));
#26188=CARTESIAN_POINT('',(688.504,-15.3685860344075,-125.));
#26189=CARTESIAN_POINT('',(688.504,-15.3685860344075,-125.));
#26190=CARTESIAN_POINT('',(688.504,-15.3685860344075,125.));
#26191=CARTESIAN_POINT('',(688.504,-15.3685860344075,125.));
#26192=CARTESIAN_POINT('',(688.504,-15.3685860344075,125.));
#26193=CARTESIAN_POINT('Origin',(695.362,-15.3685860344075,125.));
#26194=CARTESIAN_POINT('',(694.23447172088,-8.60390984261643,-125.));
#26195=CARTESIAN_POINT('Origin',(695.362,-15.3685860344075,-125.));
#26196=CARTESIAN_POINT('',(694.23447172088,-8.60390984261643,125.));
#26197=CARTESIAN_POINT('',(694.23447172088,-8.60390984261643,125.));
#26198=CARTESIAN_POINT('Origin',(695.362,-15.3685860344075,125.));
#26199=CARTESIAN_POINT('Origin',(694.23447172088,-8.60390984261643,125.));
#26200=CARTESIAN_POINT('',(717.877603066341,-4.66310049075127,-125.));
#26201=CARTESIAN_POINT('',(694.23447172088,-8.60390984261643,-125.));
#26202=CARTESIAN_POINT('',(717.877603066341,-4.66310049075127,125.));
#26203=CARTESIAN_POINT('',(717.877603066341,-4.66310049075127,125.));
#26204=CARTESIAN_POINT('',(694.23447172088,-8.60390984261643,125.));
#26205=CARTESIAN_POINT('Origin',(717.46,-2.15766486416198,125.));
#26206=CARTESIAN_POINT('',(720.,-2.15766486416198,-125.));
#26207=CARTESIAN_POINT('Origin',(717.46,-2.15766486416198,-125.));
#26208=CARTESIAN_POINT('',(720.,-2.15766486416198,125.));
#26209=CARTESIAN_POINT('',(720.,-2.15766486416198,125.));
#26210=CARTESIAN_POINT('Origin',(717.46,-2.15766486416198,125.));
#26211=CARTESIAN_POINT('Origin',(720.,0.,125.));
#26212=CARTESIAN_POINT('',(720.,0.,-125.));
#26213=CARTESIAN_POINT('',(720.,0.,-125.));
#26214=CARTESIAN_POINT('',(720.,0.,125.));
#26215=CARTESIAN_POINT('',(720.,0.,125.));
#26216=CARTESIAN_POINT('',(720.,0.,125.));
#26217=CARTESIAN_POINT('Origin',(681.9508,0.,125.));
#26218=CARTESIAN_POINT('',(681.9508,0.,-125.));
#26219=CARTESIAN_POINT('',(681.9508,0.,-125.));
#26220=CARTESIAN_POINT('',(681.9508,0.,125.));
#26221=CARTESIAN_POINT('',(681.9508,0.,125.));
#26222=CARTESIAN_POINT('',(681.9508,0.,125.));
#26223=CARTESIAN_POINT('Origin',(681.9508,-76.2,125.));
#26224=CARTESIAN_POINT('',(681.9508,-76.2,-125.));
#26225=CARTESIAN_POINT('',(681.9508,-76.2,125.));
#26226=CARTESIAN_POINT('Origin',(720.,-76.2,125.));
#26227=CARTESIAN_POINT('Origin',(720.,0.,-125.));
#26228=CARTESIAN_POINT('Origin',(38.0491999999999,-76.2,-180.));
#26229=CARTESIAN_POINT('',(38.0491999999999,-74.042335135838,-180.));
#26230=CARTESIAN_POINT('',(38.0491999999999,-76.2,-180.));
#26231=CARTESIAN_POINT('',(38.0491999999999,-76.2,-180.));
#26232=CARTESIAN_POINT('',(38.0492,-76.2,-141.9508));
#26233=CARTESIAN_POINT('',(38.0491999999999,-76.2,-180.));
#26234=CARTESIAN_POINT('',(38.0491999999999,-1.38777878078145E-14,-141.9508));
#26235=CARTESIAN_POINT('',(38.0492,-76.2,-141.9508));
#26236=CARTESIAN_POINT('',(38.0491999999999,-6.93889390390723E-15,-180.));
#26237=CARTESIAN_POINT('',(38.0491999999999,-6.93889390390723E-15,-180.));
#26238=CARTESIAN_POINT('',(38.0491999999999,-2.15766486416197,-180.));
#26239=CARTESIAN_POINT('',(38.0491999999999,-6.93889390390723E-15,-180.));
#26240=CARTESIAN_POINT('',(38.0491999999999,-4.66310049075126,-177.877603066341));
#26241=CARTESIAN_POINT('Origin',(38.0491999999999,-2.15766486416196,-177.46));
#26242=CARTESIAN_POINT('',(38.0491999999999,-8.60390984261643,-154.23447172088));
#26243=CARTESIAN_POINT('',(38.0491999999999,-8.60390984261643,-154.23447172088));
#26244=CARTESIAN_POINT('',(38.0491999999999,-15.3685860344075,-148.504));
#26245=CARTESIAN_POINT('Origin',(38.0491999999998,-15.3685860344075,-155.362));
#26246=CARTESIAN_POINT('',(38.0492,-60.8314139655925,-148.504));
#26247=CARTESIAN_POINT('',(38.0491999999999,-15.3685860344075,-148.504));
#26248=CARTESIAN_POINT('',(38.0491999999999,-67.5960901573835,-154.23447172088));
#26249=CARTESIAN_POINT('Origin',(38.0491999999998,-60.8314139655925,-155.362));
#26250=CARTESIAN_POINT('',(38.0491999999999,-71.5368995092487,-177.877603066341));
#26251=CARTESIAN_POINT('',(38.0491999999999,-67.5960901573836,-154.23447172088));
#26252=CARTESIAN_POINT('Origin',(38.0491999999999,-74.042335135838,-177.46));
#26253=CARTESIAN_POINT('Origin',(340.,-76.2,-141.9508));
#26254=CARTESIAN_POINT('',(332.282278663993,-76.2,-141.9508));
#26255=CARTESIAN_POINT('',(340.,-76.2,-141.9508));
#26256=CARTESIAN_POINT('',(332.282278663993,0.,-141.9508));
#26257=CARTESIAN_POINT('',(332.282278663993,-76.2,-141.9508));
#26258=CARTESIAN_POINT('',(340.,-6.93889390390723E-15,-141.9508));
#26259=CARTESIAN_POINT('Origin',(340.,-6.93889390390723E-15,-141.9508));
#26260=CARTESIAN_POINT('',(340.,-6.93889390390723E-15,-180.));
#26261=CARTESIAN_POINT('',(332.587255030328,-6.93889390390723E-15,-143.454366435321));
#26262=CARTESIAN_POINT('',(340.,-6.93889390390723E-15,-180.));
#26263=CARTESIAN_POINT('Origin',(340.,-6.93889390390723E-15,-180.));
#26264=CARTESIAN_POINT('',(340.,-2.15766486416197,-180.));
#26265=CARTESIAN_POINT('',(340.,-6.93889390390723E-15,-180.));
#26266=CARTESIAN_POINT('',(340.,-2.15766486416197,-180.));
#26267=CARTESIAN_POINT('Origin',(340.,-2.15766486416197,-177.46));
#26268=CARTESIAN_POINT('',(339.569502956741,-4.66310049075126,-177.877603066341));
#26269=CARTESIAN_POINT('Origin',(339.484798308677,-2.15766486416006,-177.459999999998));
#26270=CARTESIAN_POINT('',(340.,-4.66310049075127,-177.877603066341));
#26271=CARTESIAN_POINT('Origin',(340.,-8.60390984261644,-154.23447172088));
#26272=CARTESIAN_POINT('',(334.773841044404,-8.60390984261644,-154.23447172088));
#26273=CARTESIAN_POINT('',(334.974992377842,-8.43861481756234,-155.226169526879));
#26274=CARTESIAN_POINT('',(340.,-8.60390984261644,-154.23447172088));
#26275=CARTESIAN_POINT('Origin',(340.,-15.3685860344075,-155.362));
#26276=CARTESIAN_POINT('',(333.611499027604,-15.3685860344075,-148.504));
#26277=CARTESIAN_POINT('Origin',(335.002543594174,-15.3685860344061,-155.361999999998));
#26278=CARTESIAN_POINT('',(340.,-15.3685860344075,-148.504));
#26279=CARTESIAN_POINT('Origin',(340.,-15.3685860344075,-148.504));
#26280=CARTESIAN_POINT('',(333.611499027604,-60.8314139655925,-148.504));
#26281=CARTESIAN_POINT('',(333.611499027604,-15.3685860344075,-148.504));
#26282=CARTESIAN_POINT('',(340.,-60.8314139655925,-148.504));
#26283=CARTESIAN_POINT('Origin',(340.,-60.8314139655925,-155.362));
#26284=CARTESIAN_POINT('',(334.773841044404,-67.5960901573836,-154.23447172088));
#26285=CARTESIAN_POINT('Origin',(335.002543594176,-60.8314139655898,-155.362000000003));
#26286=CARTESIAN_POINT('',(340.,-67.5960901573836,-154.23447172088));
#26287=CARTESIAN_POINT('Origin',(340.,-67.5960901573836,-154.23447172088));
#26288=CARTESIAN_POINT('',(339.569502956741,-71.5368995092487,-177.877603066341));
#26289=CARTESIAN_POINT('',(334.974992377842,-67.7613851824377,-155.226169526879));
#26290=CARTESIAN_POINT('',(340.,-71.5368995092487,-177.877603066341));
#26291=CARTESIAN_POINT('Origin',(340.,-74.042335135838,-177.46));
#26292=CARTESIAN_POINT('',(340.,-74.042335135838,-180.));
#26293=CARTESIAN_POINT('Origin',(339.484798308678,-74.0423351358367,-177.460000000001));
#26294=CARTESIAN_POINT('',(340.,-74.042335135838,-180.));
#26295=CARTESIAN_POINT('Origin',(340.,-76.2,-180.));
#26296=CARTESIAN_POINT('',(340.,-76.2,-180.));
#26297=CARTESIAN_POINT('',(340.,-76.2,-180.));
#26298=CARTESIAN_POINT('',(340.,-76.2,-180.));
#26299=CARTESIAN_POINT('Origin',(340.,-76.2,-141.9508));
#26300=CARTESIAN_POINT('',(332.587255030328,-76.2,-143.454366435321));
#26301=CARTESIAN_POINT('Origin',(334.540090417271,-38.1,-153.08205587497));
#26302=CARTESIAN_POINT('Origin',(720.,-76.2,-86.9508));
#26303=CARTESIAN_POINT('',(470.,-76.2,-125.));
#26304=CARTESIAN_POINT('',(462.282278663992,-76.2,-86.9508));
#26305=CARTESIAN_POINT('',(472.466348646758,-76.2000000000001,-137.159365289908));
#26306=CARTESIAN_POINT('',(681.9508,-76.2,-125.));
#26307=CARTESIAN_POINT('',(720.,-76.2,-125.));
#26308=CARTESIAN_POINT('',(681.9508,-76.2,-86.9508));
#26309=CARTESIAN_POINT('',(681.9508,-76.2,125.));
#26310=CARTESIAN_POINT('',(720.,-76.2,-86.9508));
#26311=CARTESIAN_POINT('Origin',(720.,-76.2,-125.));
#26312=CARTESIAN_POINT('',(470.,-74.0423351358381,-125.));
#26313=CARTESIAN_POINT('',(470.,-76.2,-125.));
#26314=CARTESIAN_POINT('',(681.9508,-74.0423351358381,-125.));
#26315=CARTESIAN_POINT('',(720.,-74.0423351358381,-125.));
#26316=CARTESIAN_POINT('',(681.9508,-76.2,-125.));
#26317=CARTESIAN_POINT('Origin',(720.,-74.0423351358381,-122.46));
#26318=CARTESIAN_POINT('',(469.569502956741,-71.5368995092488,-122.877603066341));
#26319=CARTESIAN_POINT('Origin',(469.484798308677,-74.0423351358409,-122.459999999996));
#26320=CARTESIAN_POINT('',(681.9508,-71.5368995092488,-122.877603066341));
#26321=CARTESIAN_POINT('',(720.,-71.5368995092488,-122.877603066341));
#26322=CARTESIAN_POINT('Origin',(681.9508,-74.0423351358381,-122.46));
#26323=CARTESIAN_POINT('Origin',(720.,-67.5960901573836,-99.2344717208803));
#26324=CARTESIAN_POINT('',(464.773841044404,-67.5960901573836,-99.2344717208803));
#26325=CARTESIAN_POINT('',(474.597323766275,-75.6684841847121,-147.665302857156));
#26326=CARTESIAN_POINT('',(681.9508,-67.5960901573836,-99.2344717208803));
#26327=CARTESIAN_POINT('',(720.,-67.5960901573836,-99.2344717208803));
#26328=CARTESIAN_POINT('',(681.9508,-67.5960901573836,-99.2344717208803));
#26329=CARTESIAN_POINT('Origin',(720.,-60.8314139655925,-100.362));
#26330=CARTESIAN_POINT('',(463.611499027604,-60.8314139655925,-93.504));
#26331=CARTESIAN_POINT('Origin',(465.002543594174,-60.8314139655921,-100.362));
#26332=CARTESIAN_POINT('',(681.9508,-60.8314139655925,-93.504));
#26333=CARTESIAN_POINT('',(720.,-60.8314139655925,-93.504));
#26334=CARTESIAN_POINT('Origin',(681.9508,-60.8314139655925,-100.362));
#26335=CARTESIAN_POINT('Origin',(720.,-15.3685860344075,-93.504));
#26336=CARTESIAN_POINT('',(463.611499027604,-15.3685860344075,-93.504));
#26337=CARTESIAN_POINT('',(463.611499027604,-15.3685860344075,-93.504));
#26338=CARTESIAN_POINT('',(681.9508,-15.3685860344075,-93.504));
#26339=CARTESIAN_POINT('',(720.,-15.3685860344075,-93.504));
#26340=CARTESIAN_POINT('',(681.9508,-15.3685860344075,-93.504));
#26341=CARTESIAN_POINT('Origin',(720.,-15.3685860344075,-100.362));
#26342=CARTESIAN_POINT('',(464.773841044404,-8.60390984261638,-99.2344717208803));
#26343=CARTESIAN_POINT('Origin',(465.002543594173,-15.3685860344047,-100.361999999996));
#26344=CARTESIAN_POINT('',(681.9508,-8.60390984261638,-99.2344717208803));
#26345=CARTESIAN_POINT('',(720.,-8.60390984261638,-99.2344717208803));
#26346=CARTESIAN_POINT('Origin',(681.9508,-15.3685860344075,-100.362));
#26347=CARTESIAN_POINT('Origin',(720.,-8.60390984261638,-99.2344717208803));
#26348=CARTESIAN_POINT('',(469.569502956741,-4.66310049075124,-122.877603066341));
#26349=CARTESIAN_POINT('',(474.597323766275,-0.531515815287868,-147.665302857156));
#26350=CARTESIAN_POINT('',(681.9508,-4.66310049075121,-122.877603066341));
#26351=CARTESIAN_POINT('',(720.,-4.66310049075124,-122.877603066341));
#26352=CARTESIAN_POINT('',(681.9508,-8.60390984261638,-99.2344717208803));
#26353=CARTESIAN_POINT('Origin',(720.,-2.15766486416195,-122.46));
#26354=CARTESIAN_POINT('',(470.,-2.15766486416193,-125.));
#26355=CARTESIAN_POINT('Origin',(469.484798308679,-2.15766486416409,-122.460000000003));
#26356=CARTESIAN_POINT('',(681.9508,-2.15766486416192,-125.));
#26357=CARTESIAN_POINT('',(720.,-2.15766486416193,-125.));
#26358=CARTESIAN_POINT('Origin',(681.9508,-2.15766486416193,-122.46));
#26359=CARTESIAN_POINT('Origin',(720.,3.46944695195361E-14,-125.));
#26360=CARTESIAN_POINT('',(470.,2.08166817117217E-14,-125.));
#26361=CARTESIAN_POINT('',(470.,2.08166817117217E-14,-125.));
#26362=CARTESIAN_POINT('',(681.9508,4.16333634234434E-14,-125.));
#26363=CARTESIAN_POINT('',(720.,3.46944695195361E-14,-125.));
#26364=CARTESIAN_POINT('',(681.9508,4.16333634234434E-14,-125.));
#26365=CARTESIAN_POINT('Origin',(720.,2.77555756156289E-14,-86.9508));
#26366=CARTESIAN_POINT('',(462.282278663992,3.46944695195361E-14,-86.9508));
#26367=CARTESIAN_POINT('',(472.466348646758,2.77555756156289E-14,-137.159365289909));
#26368=CARTESIAN_POINT('',(681.9508,3.46944695195361E-14,-86.9508));
#26369=CARTESIAN_POINT('',(720.,2.77555756156289E-14,-86.9508));
#26370=CARTESIAN_POINT('',(681.9508,4.16333634234434E-14,125.));
#26371=CARTESIAN_POINT('Origin',(720.,-76.2,-86.9508));
#26372=CARTESIAN_POINT('',(462.282278663992,-76.2,-86.9508));
#26373=CARTESIAN_POINT('',(681.9508,-76.2,-86.9508));
#26374=CARTESIAN_POINT('Origin',(681.9508,-76.2,125.));
#26375=CARTESIAN_POINT('Origin',(464.54009041727,-38.1,-98.0820558749705));
#26376=CARTESIAN_POINT('Origin',(334.54009041727,-38.1,-153.08205587497));
#26377=CARTESIAN_POINT('',(340.,-74.042335135838,-180.));
#26378=CARTESIAN_POINT('',(340.,-76.2,-180.));
#26379=CARTESIAN_POINT('',(340.,-76.2,-180.));
#26380=CARTESIAN_POINT('',(332.282278663993,-76.2,-141.9508));
#26381=CARTESIAN_POINT('',(327.009283962863,-76.2,-115.954366435321));
#26382=CARTESIAN_POINT('',(332.282278663993,0.,-141.9508));
#26383=CARTESIAN_POINT('',(332.282278663993,-76.2,-141.9508));
#26384=CARTESIAN_POINT('',(340.,0.,-180.));
#26385=CARTESIAN_POINT('',(327.009283962863,6.93889390390723E-15,-115.954366435321));
#26386=CARTESIAN_POINT('',(340.,-2.15766486416199,-180.));
#26387=CARTESIAN_POINT('',(340.,0.,-180.));
#26388=CARTESIAN_POINT('',(339.569502956741,-4.66310049075126,-177.877603066341));
#26389=CARTESIAN_POINT('Origin',(339.484798308678,-2.15766486416058,-177.459999999999));
#26390=CARTESIAN_POINT('',(334.773841044404,-8.60390984261643,-154.23447172088));
#26391=CARTESIAN_POINT('',(329.541995367166,-12.9031508544432,-128.44090728968));
#26392=CARTESIAN_POINT('',(333.611499027604,-15.3685860344076,-148.504));
#26393=CARTESIAN_POINT('Origin',(335.002543594175,-15.3685860344113,-155.362000000004));
#26394=CARTESIAN_POINT('',(333.611499027604,-60.8314139655925,-148.504));
#26395=CARTESIAN_POINT('',(333.611499027604,-15.3685860344076,-148.504));
#26396=CARTESIAN_POINT('',(334.773841044404,-67.5960901573836,-154.23447172088));
#26397=CARTESIAN_POINT('Origin',(335.002543594174,-60.8314139655924,-155.362));
#26398=CARTESIAN_POINT('',(339.569502956741,-71.5368995092487,-177.877603066341));
#26399=CARTESIAN_POINT('',(329.541995367166,-63.2968491455568,-128.44090728968));
#26400=CARTESIAN_POINT('Origin',(339.484798308678,-74.0423351358371,-177.460000000001));
#26401=CARTESIAN_POINT('Origin',(455.174510060656,-76.2,-89.9579328706422));
#26402=CARTESIAN_POINT('',(462.282278663992,-76.2,-86.9508));
#26403=CARTESIAN_POINT('',(455.174510060656,-76.2,-89.9579328706422));
#26404=CARTESIAN_POINT('',(462.282278663992,6.93889390390723E-15,-86.9508));
#26405=CARTESIAN_POINT('',(462.282278663992,-76.2,-86.9508));
#26406=CARTESIAN_POINT('',(455.174510060656,1.38777878078145E-14,-89.9579328706422));
#26407=CARTESIAN_POINT('Origin',(455.174510060656,1.38777878078145E-14,
-89.9579328706422));
#26408=CARTESIAN_POINT('',(470.,6.93889390390723E-15,-125.));
#26409=CARTESIAN_POINT('',(462.587255030328,0.,-88.4543664353211));
#26410=CARTESIAN_POINT('',(470.,6.93889390390723E-15,-125.));
#26411=CARTESIAN_POINT('Origin',(470.,6.93889390390723E-15,-125.));
#26412=CARTESIAN_POINT('',(470.,-2.15766486416199,-125.));
#26413=CARTESIAN_POINT('',(470.,6.93889390390723E-15,-125.));
#26414=CARTESIAN_POINT('',(470.,-2.15766486416199,-125.));
#26415=CARTESIAN_POINT('Origin',(469.010314423275,-2.15766486416197,-122.660743182286));
#26416=CARTESIAN_POINT('',(469.569502956741,-4.66310049075125,-122.877603066341));
#26417=CARTESIAN_POINT('Origin',(469.484798308679,-2.15766486416551,-122.460000000004));
#26418=CARTESIAN_POINT('',(469.173029278217,-4.66310049075125,-123.045341930331));
#26419=CARTESIAN_POINT('Origin',(459.960719797421,-8.60390984261642,-101.27079224845));
#26420=CARTESIAN_POINT('',(464.773841044404,-8.60390984261643,-99.2344717208803));
#26421=CARTESIAN_POINT('',(464.974992377841,-8.43861481756233,-100.226169526879));
#26422=CARTESIAN_POINT('',(459.960719797421,-8.60390984261642,-101.27079224845));
#26423=CARTESIAN_POINT('Origin',(460.400049905766,-15.3685860344075,-102.309208868173));
#26424=CARTESIAN_POINT('',(463.611499027604,-15.3685860344075,-93.504));
#26425=CARTESIAN_POINT('Origin',(465.002543594175,-15.3685860344098,-100.362000000003));
#26426=CARTESIAN_POINT('',(457.727898848607,-15.3685860344076,-95.9932154603446));
#26427=CARTESIAN_POINT('Origin',(457.727898848607,-15.3685860344076,-95.9932154603447));
#26428=CARTESIAN_POINT('',(463.611499027604,-60.8314139655925,-93.504));
#26429=CARTESIAN_POINT('',(463.611499027604,-15.3685860344075,-93.504));
#26430=CARTESIAN_POINT('',(457.727898848607,-60.8314139655924,-95.9932154603447));
#26431=CARTESIAN_POINT('Origin',(460.400049905766,-60.8314139655924,-102.309208868173));
#26432=CARTESIAN_POINT('',(464.773841044404,-67.5960901573836,-99.2344717208803));
#26433=CARTESIAN_POINT('Origin',(465.002543594174,-60.8314139655918,-100.362000000001));
#26434=CARTESIAN_POINT('',(459.960719797421,-67.5960901573836,-101.27079224845));
#26435=CARTESIAN_POINT('Origin',(459.960719797421,-67.5960901573836,-101.27079224845));
#26436=CARTESIAN_POINT('',(469.569502956741,-71.5368995092487,-122.877603066341));
#26437=CARTESIAN_POINT('',(464.974992377841,-67.7613851824377,-100.226169526879));
#26438=CARTESIAN_POINT('',(469.173029278217,-71.5368995092487,-123.045341930331));
#26439=CARTESIAN_POINT('Origin',(469.010314423275,-74.042335135838,-122.660743182286));
#26440=CARTESIAN_POINT('',(470.,-74.042335135838,-125.));
#26441=CARTESIAN_POINT('Origin',(469.484798308679,-74.0423351358312,-122.460000000008));
#26442=CARTESIAN_POINT('',(470.,-74.042335135838,-125.));
#26443=CARTESIAN_POINT('Origin',(470.,-76.2,-125.));
#26444=CARTESIAN_POINT('',(470.,-76.2,-125.));
#26445=CARTESIAN_POINT('',(470.,-76.2,-125.));
#26446=CARTESIAN_POINT('',(470.,-76.2,-125.));
#26447=CARTESIAN_POINT('Origin',(455.174510060656,-76.2,-89.9579328706422));
#26448=CARTESIAN_POINT('',(462.587255030328,-76.2,-88.4543664353211));
#26449=CARTESIAN_POINT('Origin',(464.54009041727,-38.1,-98.0820558749704));
#26450=CARTESIAN_POINT('Origin',(254.057664864162,-9.71445146547012E-14,
144.4908));
#26451=CARTESIAN_POINT('',(251.9,-1.38777878078145E-13,180.));
#26452=CARTESIAN_POINT('',(251.9,-1.11022302462516E-13,141.9508));
#26453=CARTESIAN_POINT('',(251.9,-1.38777878078145E-13,180.));
#26454=CARTESIAN_POINT('',(254.057664864162,-8.32667268468867E-14,141.9508));
#26455=CARTESIAN_POINT('',(251.9,-1.11022302462516E-13,141.9508));
#26456=CARTESIAN_POINT('',(256.563100490752,-9.71445146547012E-14,144.073196933659));
#26457=CARTESIAN_POINT('Origin',(254.057664864162,-9.71445146547012E-14,
144.4908));
#26458=CARTESIAN_POINT('',(260.503909842617,-9.71445146547012E-14,167.716328279119));
#26459=CARTESIAN_POINT('',(260.503909842617,-9.71445146547012E-14,167.716328279119));
#26460=CARTESIAN_POINT('',(267.268586034408,-8.32667268468867E-14,173.4468));
#26461=CARTESIAN_POINT('Origin',(267.268586034408,-1.11022302462516E-13,
166.5888));
#26462=CARTESIAN_POINT('',(312.731413965592,-1.11022302462516E-13,173.4468));
#26463=CARTESIAN_POINT('',(312.731413965592,-1.11022302462516E-13,173.4468));
#26464=CARTESIAN_POINT('',(319.496090157384,-8.32667268468867E-14,167.71632827912));
#26465=CARTESIAN_POINT('Origin',(312.731413965593,-5.55111512312578E-14,
166.5888));
#26466=CARTESIAN_POINT('',(323.436899509249,-9.71445146547012E-14,144.07319693366));
#26467=CARTESIAN_POINT('',(319.496090157384,-8.32667268468867E-14,167.71632827912));
#26468=CARTESIAN_POINT('',(325.942335135838,-1.11022302462516E-13,141.9508));
#26469=CARTESIAN_POINT('Origin',(325.942335135838,-8.32667268468867E-14,
144.4908));
#26470=CARTESIAN_POINT('',(328.1,-9.71445146547012E-14,141.9508));
#26471=CARTESIAN_POINT('',(328.1,-9.71445146547012E-14,141.9508));
#26472=CARTESIAN_POINT('',(328.1,-1.11022302462516E-13,180.));
#26473=CARTESIAN_POINT('',(328.1,-1.11022302462516E-13,180.));
#26474=CARTESIAN_POINT('',(251.9,-1.38777878078145E-13,180.));
#26475=CARTESIAN_POINT('Origin',(251.9,-1.38777878078145E-13,180.));
#26476=CARTESIAN_POINT('',(328.1,150.200000000001,180.));
#26477=CARTESIAN_POINT('',(328.1,-1.11022302462516E-13,180.));
#26478=CARTESIAN_POINT('',(251.9,150.2,180.));
#26479=CARTESIAN_POINT('',(251.899999999998,150.2,180.));
#26480=CARTESIAN_POINT('',(251.9,-1.38777878078145E-13,180.));
#26481=CARTESIAN_POINT('Origin',(328.1,-1.11022302462516E-13,180.));
#26482=CARTESIAN_POINT('',(328.1,112.1508,141.9508));
#26483=CARTESIAN_POINT('',(328.1,-9.71445146547012E-14,141.9508));
#26484=CARTESIAN_POINT('',(328.100000000001,75.1000000000002,104.9));
#26485=CARTESIAN_POINT('Origin',(328.1,-9.71445146547012E-14,141.9508));
#26486=CARTESIAN_POINT('',(325.942335135838,112.1508,141.9508));
#26487=CARTESIAN_POINT('',(325.942335135838,-1.11022302462516E-13,141.9508));
#26488=CARTESIAN_POINT('',(328.1,112.1508,141.9508));
#26489=CARTESIAN_POINT('Origin',(325.942335135838,-8.32667268468867E-14,
144.4908));
#26490=CARTESIAN_POINT('',(323.436899509249,114.27319693366,144.07319693366));
#26491=CARTESIAN_POINT('',(323.436899509249,-9.71445146547012E-14,144.07319693366));
#26492=CARTESIAN_POINT('Origin',(325.94233513584,114.690800000002,144.490800000002));
#26493=CARTESIAN_POINT('Origin',(319.496090157384,-8.32667268468867E-14,
167.71632827912));
#26494=CARTESIAN_POINT('',(319.496090157384,137.91632827912,167.71632827912));
#26495=CARTESIAN_POINT('',(319.496090157384,-8.32667268468867E-14,167.71632827912));
#26496=CARTESIAN_POINT('',(330.832483055846,69.9029324635591,99.7029324635591));
#26497=CARTESIAN_POINT('Origin',(312.731413965593,-5.55111512312578E-14,
166.5888));
#26498=CARTESIAN_POINT('',(312.731413965592,143.6468,173.4468));
#26499=CARTESIAN_POINT('',(312.731413965592,-1.11022302462516E-13,173.4468));
#26500=CARTESIAN_POINT('Origin',(312.731413965592,136.788799999999,166.588799999999));
#26501=CARTESIAN_POINT('Origin',(312.731413965592,-1.11022302462516E-13,
173.4468));
#26502=CARTESIAN_POINT('',(267.268586034408,143.6468,173.4468));
#26503=CARTESIAN_POINT('',(267.268586034408,-8.32667268468867E-14,173.4468));
#26504=CARTESIAN_POINT('',(312.731413965591,143.6468,173.4468));
#26505=CARTESIAN_POINT('Origin',(267.268586034408,-1.11022302462516E-13,
166.5888));
#26506=CARTESIAN_POINT('',(260.503909842617,137.91632827912,167.716328279119));
#26507=CARTESIAN_POINT('',(260.503909842617,-9.71445146547012E-14,167.716328279119));
#26508=CARTESIAN_POINT('Origin',(267.268586034407,136.788800000001,166.5888));
#26509=CARTESIAN_POINT('Origin',(260.503909842617,-9.71445146547012E-14,
167.716328279119));
#26510=CARTESIAN_POINT('',(256.563100490752,114.273196933659,144.073196933659));
#26511=CARTESIAN_POINT('',(256.563100490752,-9.71445146547012E-14,144.073196933659));
#26512=CARTESIAN_POINT('',(249.167516944156,69.9029324635586,99.7029324635585));
#26513=CARTESIAN_POINT('Origin',(254.057664864162,-9.71445146547012E-14,
144.4908));
#26514=CARTESIAN_POINT('',(254.057664864162,112.1508,141.9508));
#26515=CARTESIAN_POINT('',(254.057664864162,-8.32667268468867E-14,141.9508));
#26516=CARTESIAN_POINT('Origin',(254.057664864162,114.6908,144.4908));
#26517=CARTESIAN_POINT('Origin',(251.9,-1.11022302462516E-13,141.9508));
#26518=CARTESIAN_POINT('',(251.9,112.1508,141.9508));
#26519=CARTESIAN_POINT('',(251.9,-1.11022302462516E-13,141.9508));
#26520=CARTESIAN_POINT('',(251.9,112.1508,141.9508));
#26521=CARTESIAN_POINT('Origin',(251.9,-1.38777878078145E-13,180.));
#26522=CARTESIAN_POINT('',(251.900000000001,75.0999999999998,104.9));
#26523=CARTESIAN_POINT('Origin',(290.,139.06874412503,168.86874412503));
#26524=CARTESIAN_POINT('Origin',(254.057664864162,-6.93889390390723E-14,
-144.4908));
#26525=CARTESIAN_POINT('',(251.9,-6.93889390390723E-14,-180.));
#26526=CARTESIAN_POINT('',(251.9,-6.93889390390723E-14,-141.9508));
#26527=CARTESIAN_POINT('',(251.9,-6.93889390390723E-14,-180.));
#26528=CARTESIAN_POINT('',(328.1,-2.77555756156289E-14,-180.));
#26529=CARTESIAN_POINT('',(251.9,-6.93889390390723E-14,-180.));
#26530=CARTESIAN_POINT('',(328.100000000001,-2.77555756156289E-14,-141.9508));
#26531=CARTESIAN_POINT('',(328.1,-2.77555756156289E-14,-180.));
#26532=CARTESIAN_POINT('',(325.942335135839,-8.32667268468867E-14,-141.9508));
#26533=CARTESIAN_POINT('',(328.100000000001,-2.77555756156289E-14,-141.9508));
#26534=CARTESIAN_POINT('',(323.436899509249,-2.77555756156289E-14,-144.07319693366));
#26535=CARTESIAN_POINT('Origin',(325.942335135839,-5.55111512312578E-14,
-144.4908));
#26536=CARTESIAN_POINT('',(319.496090157384,-5.55111512312578E-14,-167.71632827912));
#26537=CARTESIAN_POINT('',(319.496090157384,-5.55111512312578E-14,-167.71632827912));
#26538=CARTESIAN_POINT('',(312.731413965593,-4.16333634234434E-14,-173.4468));
#26539=CARTESIAN_POINT('Origin',(312.731413965593,-5.55111512312578E-14,
-166.5888));
#26540=CARTESIAN_POINT('',(267.268586034408,-1.38777878078145E-14,-173.4468));
#26541=CARTESIAN_POINT('',(312.731413965593,-4.16333634234434E-14,-173.4468));
#26542=CARTESIAN_POINT('',(260.503909842617,-1.38777878078145E-14,-167.71632827912));
#26543=CARTESIAN_POINT('Origin',(267.268586034408,-5.55111512312578E-14,
-166.5888));
#26544=CARTESIAN_POINT('',(256.563100490752,-8.32667268468867E-14,-144.073196933659));
#26545=CARTESIAN_POINT('',(260.503909842617,-1.38777878078145E-14,-167.71632827912));
#26546=CARTESIAN_POINT('',(254.057664864163,-4.16333634234434E-14,-141.9508));
#26547=CARTESIAN_POINT('Origin',(254.057664864162,-6.93889390390723E-14,
-144.4908));
#26548=CARTESIAN_POINT('',(251.9,-6.93889390390723E-14,-141.9508));
#26549=CARTESIAN_POINT('Origin',(251.9,150.2,-180.));
#26550=CARTESIAN_POINT('',(251.9,150.2,-180.));
#26551=CARTESIAN_POINT('',(251.9,150.2,-180.));
#26552=CARTESIAN_POINT('',(328.1,150.2,-180.));
#26553=CARTESIAN_POINT('',(251.9,150.2,-180.));
#26554=CARTESIAN_POINT('',(328.1,150.2,-180.));
#26555=CARTESIAN_POINT('Origin',(328.1,150.2,-180.));
#26556=CARTESIAN_POINT('',(328.100000000001,112.1508,-141.9508));
#26557=CARTESIAN_POINT('',(328.1,150.2,-180.));
#26558=CARTESIAN_POINT('',(328.100000000001,150.2,-141.9508));
#26559=CARTESIAN_POINT('Origin',(328.100000000001,150.2,-141.9508));
#26560=CARTESIAN_POINT('',(325.942335135839,112.1508,-141.9508));
#26561=CARTESIAN_POINT('',(328.100000000001,112.1508,-141.9508));
#26562=CARTESIAN_POINT('',(325.942335135839,150.2,-141.9508));
#26563=CARTESIAN_POINT('Origin',(325.942335135839,150.2,-144.4908));
#26564=CARTESIAN_POINT('',(323.436899509249,114.27319693366,-144.07319693366));
#26565=CARTESIAN_POINT('Origin',(325.942335135836,114.690799999997,-144.490799999997));
#26566=CARTESIAN_POINT('',(323.436899509249,150.2,-144.07319693366));
#26567=CARTESIAN_POINT('Origin',(319.496090157384,150.2,-167.71632827912));
#26568=CARTESIAN_POINT('',(319.496090157384,137.91632827912,-167.71632827912));
#26569=CARTESIAN_POINT('',(318.48640167016,143.974017294229,-173.774017294229));
#26570=CARTESIAN_POINT('',(319.496090157384,150.2,-167.71632827912));
#26571=CARTESIAN_POINT('Origin',(312.731413965593,150.2,-166.5888));
#26572=CARTESIAN_POINT('',(312.731413965593,143.6468,-173.4468));
#26573=CARTESIAN_POINT('Origin',(312.7314139656,136.788800000009,-166.588800000009));
#26574=CARTESIAN_POINT('',(312.731413965593,150.2,-173.4468));
#26575=CARTESIAN_POINT('Origin',(312.731413965593,150.2,-173.4468));
#26576=CARTESIAN_POINT('',(267.268586034408,143.6468,-173.4468));
#26577=CARTESIAN_POINT('',(312.731413965593,143.6468,-173.4468));
#26578=CARTESIAN_POINT('',(267.268586034408,150.2,-173.4468));
#26579=CARTESIAN_POINT('Origin',(267.268586034408,150.2,-166.5888));
#26580=CARTESIAN_POINT('',(260.503909842617,137.916328279119,-167.71632827912));
#26581=CARTESIAN_POINT('Origin',(267.268586034409,136.788799999999,-166.588799999999));
#26582=CARTESIAN_POINT('',(260.503909842617,150.2,-167.71632827912));
#26583=CARTESIAN_POINT('Origin',(260.503909842617,150.2,-167.71632827912));
#26584=CARTESIAN_POINT('',(256.563100490752,114.273196933659,-144.073196933659));
#26585=CARTESIAN_POINT('',(261.51359832984,143.974017294229,-173.774017294229));
#26586=CARTESIAN_POINT('',(256.563100490752,150.2,-144.073196933659));
#26587=CARTESIAN_POINT('Origin',(254.057664864162,150.2,-144.4908));
#26588=CARTESIAN_POINT('',(254.057664864163,112.1508,-141.9508));
#26589=CARTESIAN_POINT('Origin',(254.057664864164,114.690799999997,-144.490799999997));
#26590=CARTESIAN_POINT('',(254.057664864163,150.2,-141.9508));
#26591=CARTESIAN_POINT('Origin',(251.9,150.2,-141.9508));
#26592=CARTESIAN_POINT('',(251.9,112.1508,-141.9508));
#26593=CARTESIAN_POINT('',(251.9,112.1508,-141.9508));
#26594=CARTESIAN_POINT('',(251.9,150.2,-141.9508));
#26595=CARTESIAN_POINT('Origin',(251.9,150.2,-180.));
#26596=CARTESIAN_POINT('',(251.9,150.2,-180.));
#26597=CARTESIAN_POINT('Origin',(290.,139.06874412503,-168.86874412503));
#26598=CARTESIAN_POINT('Origin',(9.99492,80.,180.));
#26599=CARTESIAN_POINT('',(9.99491999999973,-6.93889390390723E-15,154.6));
#26600=CARTESIAN_POINT('',(9.99491999999999,6.93889390390723E-15,180.));
#26601=CARTESIAN_POINT('',(9.99491999999999,6.93889390390723E-15,180.));
#26602=CARTESIAN_POINT('',(9.99492,80.,180.));
#26603=CARTESIAN_POINT('',(9.99492,80.,180.));
#26604=CARTESIAN_POINT('',(9.99491999999973,80.,154.6));
#26605=CARTESIAN_POINT('',(9.99492,80.,180.));
#26606=CARTESIAN_POINT('',(9.99491999999973,80.,154.6));
#26607=CARTESIAN_POINT('Origin',(10.,80.,180.));
#26608=CARTESIAN_POINT('',(10.,6.93889390390723E-15,180.));
#26609=CARTESIAN_POINT('',(10.,6.93889390390723E-15,180.));
#26610=CARTESIAN_POINT('',(10.,80.,180.));
#26611=CARTESIAN_POINT('',(10.,80.,180.));
#26612=CARTESIAN_POINT('',(10.,80.,180.));
#26613=CARTESIAN_POINT('Origin',(9.99999999999996,80.,176.83008));
#26614=CARTESIAN_POINT('',(13.16992,-1.38777878078145E-14,176.83008));
#26615=CARTESIAN_POINT('Origin',(9.99999999999996,-1.38777878078145E-14,
176.83008));
#26616=CARTESIAN_POINT('',(13.16992,80.,176.83008));
#26617=CARTESIAN_POINT('',(13.16992,80.,176.83008));
#26618=CARTESIAN_POINT('Origin',(9.99999999999996,80.,176.83008));
#26619=CARTESIAN_POINT('Origin',(13.1699199999998,80.,162.5375));
#26620=CARTESIAN_POINT('',(13.1699199999998,-6.93889390390723E-15,162.5375));
#26621=CARTESIAN_POINT('',(13.1699199999998,-6.93889390390723E-15,162.5375));
#26622=CARTESIAN_POINT('',(13.1699199999998,80.,162.5375));
#26623=CARTESIAN_POINT('',(13.1699199999998,80.,162.5375));
#26624=CARTESIAN_POINT('',(13.1699199999998,80.,162.5375));
#26625=CARTESIAN_POINT('Origin',(17.9324199999998,80.,162.5375));
#26626=CARTESIAN_POINT('',(17.9324199999998,-6.93889390390723E-15,157.775));
#26627=CARTESIAN_POINT('Origin',(17.9324199999998,-6.93889390390723E-15,
162.5375));
#26628=CARTESIAN_POINT('',(17.9324199999998,80.,157.775));
#26629=CARTESIAN_POINT('',(17.9324199999998,80.,157.775));
#26630=CARTESIAN_POINT('Origin',(17.9324199999998,80.,162.5375));
#26631=CARTESIAN_POINT('Origin',(32.2249999999998,80.,157.775));
#26632=CARTESIAN_POINT('',(32.2249999999998,-6.93889390390723E-15,157.775));
#26633=CARTESIAN_POINT('',(32.2249999999998,-6.93889390390723E-15,157.775));
#26634=CARTESIAN_POINT('',(32.2249999999998,80.,157.775));
#26635=CARTESIAN_POINT('',(32.2249999999998,80.,157.775));
#26636=CARTESIAN_POINT('',(32.2249999999998,80.,157.775));
#26637=CARTESIAN_POINT('Origin',(32.2249999999997,80.,154.60508));
#26638=CARTESIAN_POINT('',(35.3949199999997,-2.08166817117217E-14,154.60508));
#26639=CARTESIAN_POINT('Origin',(32.2249999999997,-1.38777878078145E-14,
154.60508));
#26640=CARTESIAN_POINT('',(35.3949199999997,80.,154.60508));
#26641=CARTESIAN_POINT('',(35.3949199999997,80.,154.60508));
#26642=CARTESIAN_POINT('Origin',(32.2249999999997,80.,154.60508));
#26643=CARTESIAN_POINT('Origin',(35.3949199999997,80.,154.6));
#26644=CARTESIAN_POINT('',(35.3949199999997,-2.08166817117217E-14,154.6));
#26645=CARTESIAN_POINT('',(35.3949199999997,-2.08166817117217E-14,154.6));
#26646=CARTESIAN_POINT('',(35.3949199999997,80.,154.6));
#26647=CARTESIAN_POINT('',(35.3949199999997,80.,154.6));
#26648=CARTESIAN_POINT('',(35.3949199999997,80.,154.6));
#26649=CARTESIAN_POINT('Origin',(9.99491999999973,80.,154.6));
#26650=CARTESIAN_POINT('',(9.99491999999973,-6.93889390390723E-15,154.6));
#26651=CARTESIAN_POINT('',(9.99491999999973,80.,154.6));
#26652=CARTESIAN_POINT('Origin',(32.2249999999997,80.,154.60508));
#26653=CARTESIAN_POINT('Origin',(32.2249999999997,-1.38777878078145E-14,
154.60508));
#26654=CARTESIAN_POINT('Origin',(210.00508,4.16333634234434E-14,180.));
#26655=CARTESIAN_POINT('',(210.00508,80.,154.6));
#26656=CARTESIAN_POINT('',(210.00508,80.0000000000001,180.));
#26657=CARTESIAN_POINT('',(210.00508,80.0000000000001,180.));
#26658=CARTESIAN_POINT('',(210.00508,4.16333634234434E-14,180.));
#26659=CARTESIAN_POINT('',(210.00508,4.16333634234434E-14,180.));
#26660=CARTESIAN_POINT('',(210.00508,1.38777878078145E-14,154.6));
#26661=CARTESIAN_POINT('',(210.00508,4.16333634234434E-14,180.));
#26662=CARTESIAN_POINT('',(210.00508,1.38777878078145E-14,154.6));
#26663=CARTESIAN_POINT('Origin',(210.,4.16333634234434E-14,180.));
#26664=CARTESIAN_POINT('',(210.,80.0000000000001,180.));
#26665=CARTESIAN_POINT('',(210.,80.0000000000001,180.));
#26666=CARTESIAN_POINT('',(210.,4.16333634234434E-14,180.));
#26667=CARTESIAN_POINT('',(210.,4.16333634234434E-14,180.));
#26668=CARTESIAN_POINT('',(210.,4.16333634234434E-14,180.));
#26669=CARTESIAN_POINT('Origin',(210.,2.08166817117217E-14,176.83008));
#26670=CARTESIAN_POINT('',(206.83008,80.0000000000001,176.83008));
#26671=CARTESIAN_POINT('Origin',(210.,80.,176.83008));
#26672=CARTESIAN_POINT('',(206.83008,4.85722573273506E-14,176.83008));
#26673=CARTESIAN_POINT('',(206.83008,4.85722573273506E-14,176.83008));
#26674=CARTESIAN_POINT('Origin',(210.,2.08166817117217E-14,176.83008));
#26675=CARTESIAN_POINT('Origin',(206.83008,2.77555756156289E-14,162.5375));
#26676=CARTESIAN_POINT('',(206.83008,80.,162.5375));
#26677=CARTESIAN_POINT('',(206.83008,80.,162.5375));
#26678=CARTESIAN_POINT('',(206.83008,2.77555756156289E-14,162.5375));
#26679=CARTESIAN_POINT('',(206.83008,2.77555756156289E-14,162.5375));
#26680=CARTESIAN_POINT('',(206.83008,2.77555756156289E-14,162.5375));
#26681=CARTESIAN_POINT('Origin',(202.06758,2.77555756156289E-14,162.5375));
#26682=CARTESIAN_POINT('',(202.06758,80.,157.775));
#26683=CARTESIAN_POINT('Origin',(202.06758,80.,162.5375));
#26684=CARTESIAN_POINT('',(202.06758,2.77555756156289E-14,157.775));
#26685=CARTESIAN_POINT('',(202.06758,2.77555756156289E-14,157.775));
#26686=CARTESIAN_POINT('Origin',(202.06758,2.77555756156289E-14,162.5375));
#26687=CARTESIAN_POINT('Origin',(187.775,2.77555756156289E-14,157.775));
#26688=CARTESIAN_POINT('',(187.775,80.,157.775));
#26689=CARTESIAN_POINT('',(187.775,80.,157.775));
#26690=CARTESIAN_POINT('',(187.775,2.77555756156289E-14,157.775));
#26691=CARTESIAN_POINT('',(187.775,2.77555756156289E-14,157.775));
#26692=CARTESIAN_POINT('',(187.775,2.77555756156289E-14,157.775));
#26693=CARTESIAN_POINT('Origin',(187.775,1.38777878078145E-14,154.60508));
#26694=CARTESIAN_POINT('',(184.60508,80.,154.60508));
#26695=CARTESIAN_POINT('Origin',(187.775,80.,154.60508));
#26696=CARTESIAN_POINT('',(184.60508,4.16333634234434E-14,154.60508));
#26697=CARTESIAN_POINT('',(184.60508,4.16333634234434E-14,154.60508));
#26698=CARTESIAN_POINT('Origin',(187.775,1.38777878078145E-14,154.60508));
#26699=CARTESIAN_POINT('Origin',(184.60508,4.16333634234434E-14,154.6));
#26700=CARTESIAN_POINT('',(184.60508,80.,154.6));
#26701=CARTESIAN_POINT('',(184.60508,80.,154.6));
#26702=CARTESIAN_POINT('',(184.60508,4.16333634234434E-14,154.6));
#26703=CARTESIAN_POINT('',(184.60508,4.16333634234434E-14,154.6));
#26704=CARTESIAN_POINT('',(184.60508,4.16333634234434E-14,154.6));
#26705=CARTESIAN_POINT('Origin',(210.00508,1.38777878078145E-14,154.6));
#26706=CARTESIAN_POINT('',(210.00508,80.,154.6));
#26707=CARTESIAN_POINT('',(210.00508,1.38777878078145E-14,154.6));
#26708=CARTESIAN_POINT('Origin',(187.775,1.38777878078145E-14,154.60508));
#26709=CARTESIAN_POINT('Origin',(187.775,80.,154.60508));
#26710=CARTESIAN_POINT('Origin',(9.99492,80.,-180.));
#26711=CARTESIAN_POINT('',(9.99491999999973,-9.72456449527445E-15,-154.6));
#26712=CARTESIAN_POINT('',(9.99492,4.62223186652937E-30,-180.));
#26713=CARTESIAN_POINT('',(9.99492,4.62223186652937E-30,-180.));
#26714=CARTESIAN_POINT('',(9.99491999999973,80.,-154.6));
#26715=CARTESIAN_POINT('',(9.99491999999973,80.,-154.6));
#26716=CARTESIAN_POINT('',(9.99492,80.,-180.));
#26717=CARTESIAN_POINT('',(9.99492,80.,-180.));
#26718=CARTESIAN_POINT('',(9.99492,80.,-180.));
#26719=CARTESIAN_POINT('Origin',(10.,80.,-180.));
#26720=CARTESIAN_POINT('',(10.,3.08148791101958E-30,-180.));
#26721=CARTESIAN_POINT('',(10.,4.62223186652937E-30,-180.));
#26722=CARTESIAN_POINT('',(10.,80.,-180.));
#26723=CARTESIAN_POINT('',(10.,80.,-180.));
#26724=CARTESIAN_POINT('',(10.,80.,-180.));
#26725=CARTESIAN_POINT('Origin',(9.99999999999996,80.,-176.83008));
#26726=CARTESIAN_POINT('',(13.16992,-1.21362564901026E-15,-176.83008));
#26727=CARTESIAN_POINT('Origin',(9.99999999999996,-1.21362564901025E-15,
-176.83008));
#26728=CARTESIAN_POINT('',(13.16992,80.,-176.83008));
#26729=CARTESIAN_POINT('Origin',(9.99999999999996,80.,-176.83008));
#26730=CARTESIAN_POINT('',(13.16992,80.,-176.83008));
#26731=CARTESIAN_POINT('Origin',(13.1699199999998,80.,-162.5375));
#26732=CARTESIAN_POINT('',(13.1699199999998,-6.68563809050119E-15,-162.5375));
#26733=CARTESIAN_POINT('',(13.1699199999998,-6.68563809050119E-15,-162.5375));
#26734=CARTESIAN_POINT('',(13.1699199999998,80.,-162.5375));
#26735=CARTESIAN_POINT('',(13.1699199999998,80.,-162.5375));
#26736=CARTESIAN_POINT('',(13.1699199999998,80.,-162.5375));
#26737=CARTESIAN_POINT('Origin',(17.9324199999998,80.,-162.5375));
#26738=CARTESIAN_POINT('',(17.9324199999998,-8.50899393336517E-15,-157.775));
#26739=CARTESIAN_POINT('Origin',(17.9324199999998,-6.68563809050121E-15,
-162.5375));
#26740=CARTESIAN_POINT('',(17.9324199999998,80.,-157.775));
#26741=CARTESIAN_POINT('Origin',(17.9324199999998,80.,-162.5375));
#26742=CARTESIAN_POINT('',(17.9324199999998,80.,-157.775));
#26743=CARTESIAN_POINT('Origin',(32.2249999999998,80.,-157.775));
#26744=CARTESIAN_POINT('',(32.2249999999998,-8.50899393336523E-15,-157.775));
#26745=CARTESIAN_POINT('',(32.2249999999998,-8.50899393336523E-15,-157.775));
#26746=CARTESIAN_POINT('',(32.2249999999998,80.,-157.775));
#26747=CARTESIAN_POINT('',(32.2249999999998,80.,-157.775));
#26748=CARTESIAN_POINT('',(32.2249999999998,80.,-157.775));
#26749=CARTESIAN_POINT('Origin',(32.2249999999997,80.,-154.60508));
#26750=CARTESIAN_POINT('',(35.3949199999997,-9.72261958237549E-15,-154.60508));
#26751=CARTESIAN_POINT('Origin',(32.2249999999997,-9.72261958237548E-15,
-154.60508));
#26752=CARTESIAN_POINT('',(35.3949199999997,80.,-154.60508));
#26753=CARTESIAN_POINT('Origin',(32.2249999999997,80.,-154.60508));
#26754=CARTESIAN_POINT('',(35.3949199999997,80.,-154.60508));
#26755=CARTESIAN_POINT('Origin',(35.3949199999997,80.,-154.6));
#26756=CARTESIAN_POINT('',(35.3949199999997,-9.72456449527455E-15,-154.6));
#26757=CARTESIAN_POINT('',(35.3949199999997,-9.72456449527455E-15,-154.6));
#26758=CARTESIAN_POINT('',(35.3949199999997,80.,-154.6));
#26759=CARTESIAN_POINT('',(35.3949199999997,80.,-154.6));
#26760=CARTESIAN_POINT('',(35.3949199999997,80.,-154.6));
#26761=CARTESIAN_POINT('Origin',(9.99491999999973,80.,-154.6));
#26762=CARTESIAN_POINT('',(9.99491999999973,-9.72456449527445E-15,-154.6));
#26763=CARTESIAN_POINT('',(9.99491999999973,80.,-154.6));
#26764=CARTESIAN_POINT('Origin',(32.2249999999997,80.,-154.60508));
#26765=CARTESIAN_POINT('Origin',(32.2249999999997,-9.72261958237548E-15,
-154.60508));
#26766=CARTESIAN_POINT('Origin',(210.00508,4.16333634234434E-14,-180.));
#26767=CARTESIAN_POINT('',(210.00508,80.,-154.6));
#26768=CARTESIAN_POINT('',(210.00508,80.0000000000001,-180.));
#26769=CARTESIAN_POINT('',(210.00508,80.0000000000001,-180.));
#26770=CARTESIAN_POINT('',(210.00508,1.38777878078145E-14,-154.6));
#26771=CARTESIAN_POINT('',(210.00508,1.38777878078145E-14,-154.6));
#26772=CARTESIAN_POINT('',(210.00508,4.16333634234434E-14,-180.));
#26773=CARTESIAN_POINT('',(210.00508,4.16333634234434E-14,-180.));
#26774=CARTESIAN_POINT('',(210.00508,4.16333634234434E-14,-180.));
#26775=CARTESIAN_POINT('Origin',(210.,4.16333634234434E-14,-180.));
#26776=CARTESIAN_POINT('',(210.,80.0000000000001,-180.));
#26777=CARTESIAN_POINT('',(210.,80.0000000000001,-180.));
#26778=CARTESIAN_POINT('',(210.,4.16333634234434E-14,-180.));
#26779=CARTESIAN_POINT('',(210.,4.16333634234434E-14,-180.));
#26780=CARTESIAN_POINT('',(210.,4.16333634234434E-14,-180.));
#26781=CARTESIAN_POINT('Origin',(210.,2.77555756156289E-14,-176.83008));
#26782=CARTESIAN_POINT('',(206.83008,80.,-176.83008));
#26783=CARTESIAN_POINT('Origin',(210.,80.,-176.83008));
#26784=CARTESIAN_POINT('',(206.83008,2.77555756156289E-14,-176.83008));
#26785=CARTESIAN_POINT('Origin',(210.,2.77555756156289E-14,-176.83008));
#26786=CARTESIAN_POINT('',(206.83008,2.77555756156289E-14,-176.83008));
#26787=CARTESIAN_POINT('Origin',(206.83008,2.77555756156289E-14,-162.5375));
#26788=CARTESIAN_POINT('',(206.83008,80.,-162.5375));
#26789=CARTESIAN_POINT('',(206.83008,80.,-162.5375));
#26790=CARTESIAN_POINT('',(206.83008,2.77555756156289E-14,-162.5375));
#26791=CARTESIAN_POINT('',(206.83008,2.77555756156289E-14,-162.5375));
#26792=CARTESIAN_POINT('',(206.83008,2.77555756156289E-14,-162.5375));
#26793=CARTESIAN_POINT('Origin',(202.06758,2.77555756156289E-14,-162.5375));
#26794=CARTESIAN_POINT('',(202.06758,80.,-157.775));
#26795=CARTESIAN_POINT('Origin',(202.06758,80.,-162.5375));
#26796=CARTESIAN_POINT('',(202.06758,1.38777878078145E-14,-157.775));
#26797=CARTESIAN_POINT('Origin',(202.06758,2.77555756156289E-14,-162.5375));
#26798=CARTESIAN_POINT('',(202.06758,1.38777878078145E-14,-157.775));
#26799=CARTESIAN_POINT('Origin',(187.775,1.38777878078145E-14,-157.775));
#26800=CARTESIAN_POINT('',(187.775,80.,-157.775));
#26801=CARTESIAN_POINT('',(187.775,80.,-157.775));
#26802=CARTESIAN_POINT('',(187.775,1.38777878078145E-14,-157.775));
#26803=CARTESIAN_POINT('',(187.775,1.38777878078145E-14,-157.775));
#26804=CARTESIAN_POINT('',(187.775,1.38777878078145E-14,-157.775));
#26805=CARTESIAN_POINT('Origin',(187.775,1.38777878078145E-14,-154.60508));
#26806=CARTESIAN_POINT('',(184.60508,80.,-154.60508));
#26807=CARTESIAN_POINT('Origin',(187.775,80.,-154.60508));
#26808=CARTESIAN_POINT('',(184.60508,1.38777878078145E-14,-154.60508));
#26809=CARTESIAN_POINT('Origin',(187.775,1.38777878078145E-14,-154.60508));
#26810=CARTESIAN_POINT('',(184.60508,1.38777878078145E-14,-154.60508));
#26811=CARTESIAN_POINT('Origin',(184.60508,1.38777878078145E-14,-154.6));
#26812=CARTESIAN_POINT('',(184.60508,80.,-154.6));
#26813=CARTESIAN_POINT('',(184.60508,80.,-154.6));
#26814=CARTESIAN_POINT('',(184.60508,1.38777878078145E-14,-154.6));
#26815=CARTESIAN_POINT('',(184.60508,1.38777878078145E-14,-154.6));
#26816=CARTESIAN_POINT('',(184.60508,1.38777878078145E-14,-154.6));
#26817=CARTESIAN_POINT('Origin',(210.00508,1.38777878078145E-14,-154.6));
#26818=CARTESIAN_POINT('',(210.00508,80.,-154.6));
#26819=CARTESIAN_POINT('',(210.00508,1.38777878078145E-14,-154.6));
#26820=CARTESIAN_POINT('Origin',(187.775,1.38777878078145E-14,-154.60508));
#26821=CARTESIAN_POINT('Origin',(187.775,80.,-154.60508));
#26822=CARTESIAN_POINT('Origin',(502.23008,4.16333634234434E-14,124.99492));
#26823=CARTESIAN_POINT('',(480.,-1.2490009027033E-13,125.));
#26824=CARTESIAN_POINT('',(480.,-1.2490009027033E-13,99.6));
#26825=CARTESIAN_POINT('',(480.,-1.2490009027033E-13,99.6));
#26826=CARTESIAN_POINT('',(480.00508,-8.32667268468867E-14,99.6));
#26827=CARTESIAN_POINT('',(480.00508,-8.32667268468867E-14,99.6));
#26828=CARTESIAN_POINT('',(483.175,-4.16333634234434E-14,102.76992));
#26829=CARTESIAN_POINT('Origin',(480.00508,-1.2490009027033E-13,102.76992));
#26830=CARTESIAN_POINT('',(483.175,-4.16333634234434E-14,117.0625));
#26831=CARTESIAN_POINT('',(483.175,-4.16333634234434E-14,117.0625));
#26832=CARTESIAN_POINT('',(487.9375,-8.32667268468867E-14,121.825));
#26833=CARTESIAN_POINT('Origin',(487.9375,-8.32667268468867E-14,117.0625));
#26834=CARTESIAN_POINT('',(502.23008,4.16333634234434E-14,121.825));
#26835=CARTESIAN_POINT('',(502.23008,4.16333634234434E-14,121.825));
#26836=CARTESIAN_POINT('',(505.4,-4.16333634234434E-14,124.99492));
#26837=CARTESIAN_POINT('Origin',(502.23008,4.16333634234434E-14,124.99492));
#26838=CARTESIAN_POINT('',(505.4,-8.32667268468867E-14,125.));
#26839=CARTESIAN_POINT('',(505.4,-8.32667268468867E-14,125.));
#26840=CARTESIAN_POINT('',(480.,-1.2490009027033E-13,125.));
#26841=CARTESIAN_POINT('Origin',(480.,-1.2490009027033E-13,125.));
#26842=CARTESIAN_POINT('',(505.4,132.,125.));
#26843=CARTESIAN_POINT('',(505.4,-8.32667268468867E-14,125.));
#26844=CARTESIAN_POINT('',(480.,132.,125.));
#26845=CARTESIAN_POINT('',(479.999999999999,132.,125.));
#26846=CARTESIAN_POINT('',(480.,-1.2490009027033E-13,125.));
#26847=CARTESIAN_POINT('Origin',(505.4,-8.32667268468867E-14,125.));
#26848=CARTESIAN_POINT('',(505.4,131.99492,124.99492));
#26849=CARTESIAN_POINT('',(505.4,-4.16333634234434E-14,124.99492));
#26850=CARTESIAN_POINT('',(505.4,66.0000000000001,59.0000000000001));
#26851=CARTESIAN_POINT('Origin',(502.23008,4.16333634234434E-14,124.99492));
#26852=CARTESIAN_POINT('',(502.23008,128.825,121.825));
#26853=CARTESIAN_POINT('',(502.23008,4.16333634234434E-14,121.825));
#26854=CARTESIAN_POINT('Origin',(502.230079999999,131.994920000002,124.994920000002));
#26855=CARTESIAN_POINT('Origin',(502.23008,4.16333634234434E-14,121.825));
#26856=CARTESIAN_POINT('',(487.9375,128.825,121.825));
#26857=CARTESIAN_POINT('',(487.9375,-8.32667268468867E-14,121.825));
#26858=CARTESIAN_POINT('',(502.230079999999,128.825,121.825));
#26859=CARTESIAN_POINT('Origin',(487.9375,-8.32667268468867E-14,117.0625));
#26860=CARTESIAN_POINT('',(483.175,124.0625,117.0625));
#26861=CARTESIAN_POINT('',(483.175,-4.16333634234434E-14,117.0625));
#26862=CARTESIAN_POINT('Origin',(487.937500000006,124.062499999993,117.062499999993));
#26863=CARTESIAN_POINT('Origin',(483.175,-4.16333634234434E-14,117.0625));
#26864=CARTESIAN_POINT('',(483.175,109.76992,102.76992));
#26865=CARTESIAN_POINT('',(483.175,-4.16333634234434E-14,102.76992));
#26866=CARTESIAN_POINT('',(483.175000000001,62.03125,55.03125));
#26867=CARTESIAN_POINT('Origin',(480.00508,-1.2490009027033E-13,102.76992));
#26868=CARTESIAN_POINT('',(480.00508,106.6,99.6));
#26869=CARTESIAN_POINT('',(480.00508,-8.32667268468867E-14,99.6));
#26870=CARTESIAN_POINT('Origin',(480.005080000002,109.769919999998,102.769919999998));
#26871=CARTESIAN_POINT('Origin',(480.00508,-8.32667268468867E-14,99.6));
#26872=CARTESIAN_POINT('',(480.,106.6,99.6));
#26873=CARTESIAN_POINT('',(480.,-1.2490009027033E-13,99.6));
#26874=CARTESIAN_POINT('',(480.00508,106.6,99.6));
#26875=CARTESIAN_POINT('Origin',(480.,-1.2490009027033E-13,99.6));
#26876=CARTESIAN_POINT('',(480.000000000001,53.3,46.3));
#26877=CARTESIAN_POINT('Origin',(487.322189922481,124.67781007752,117.677810077519));
#26878=CARTESIAN_POINT('Origin',(480.,106.6,125.));
#26879=CARTESIAN_POINT('',(480.,106.6,-99.6));
#26880=CARTESIAN_POINT('',(480.,132.,-125.));
#26881=CARTESIAN_POINT('',(480.000000000001,-5.70000000000001,12.7));
#26882=CARTESIAN_POINT('',(480.,106.6,99.6000000000001));
#26883=CARTESIAN_POINT('',(480.,106.6,125.));
#26884=CARTESIAN_POINT('',(480.,132.,125.));
#26885=CARTESIAN_POINT('',(480.,119.3,112.3));
#26886=CARTESIAN_POINT('',(480.,132.,125.));
#26887=CARTESIAN_POINT('Origin',(480.00508,106.6,125.));
#26888=CARTESIAN_POINT('',(480.00508,106.6,-99.6000000000001));
#26889=CARTESIAN_POINT('',(480.00508,106.6,-99.6000000000001));
#26890=CARTESIAN_POINT('',(480.00508,106.6,99.6000000000001));
#26891=CARTESIAN_POINT('',(480.00508,106.6,125.));
#26892=CARTESIAN_POINT('',(480.00508,106.6,99.6000000000001));
#26893=CARTESIAN_POINT('Origin',(480.00508,109.76992,125.));
#26894=CARTESIAN_POINT('',(483.175,109.76992,-102.76992));
#26895=CARTESIAN_POINT('Origin',(480.005079999996,109.769920000004,-102.769920000004));
#26896=CARTESIAN_POINT('',(483.175,109.76992,102.76992));
#26897=CARTESIAN_POINT('',(483.175,109.76992,125.));
#26898=CARTESIAN_POINT('Origin',(480.005080000004,109.769919999996,102.769919999996));
#26899=CARTESIAN_POINT('Origin',(483.175,124.0625,125.));
#26900=CARTESIAN_POINT('',(483.175,124.0625,-117.0625));
#26901=CARTESIAN_POINT('',(483.175000000001,3.03124999999993,3.96874999999999));
#26902=CARTESIAN_POINT('',(483.175,124.0625,117.0625));
#26903=CARTESIAN_POINT('',(483.175,124.0625,125.));
#26904=CARTESIAN_POINT('',(483.175,128.03125,121.03125));
#26905=CARTESIAN_POINT('Origin',(487.9375,124.0625,125.));
#26906=CARTESIAN_POINT('',(487.9375,128.825,-121.825));
#26907=CARTESIAN_POINT('Origin',(487.9375,124.062500000001,-117.062500000001));
#26908=CARTESIAN_POINT('',(487.9375,128.825,121.825));
#26909=CARTESIAN_POINT('',(487.9375,128.825,125.));
#26910=CARTESIAN_POINT('Origin',(487.937500000005,124.062499999995,117.062499999995));
#26911=CARTESIAN_POINT('Origin',(502.23008,128.825,125.));
#26912=CARTESIAN_POINT('',(502.23008,128.825,-121.825));
#26913=CARTESIAN_POINT('',(502.230079999997,128.825,-121.825));
#26914=CARTESIAN_POINT('',(502.23008,128.825,121.825));
#26915=CARTESIAN_POINT('',(502.23008,128.825,125.));
#26916=CARTESIAN_POINT('',(502.23008,128.825,121.825));
#26917=CARTESIAN_POINT('Origin',(502.23008,131.99492,125.));
#26918=CARTESIAN_POINT('',(505.4,131.99492,-124.99492));
#26919=CARTESIAN_POINT('Origin',(502.230079999997,131.994920000003,-124.994920000003));
#26920=CARTESIAN_POINT('',(505.4,131.99492,124.99492));
#26921=CARTESIAN_POINT('',(505.4,131.99492,125.));
#26922=CARTESIAN_POINT('Origin',(502.230080000004,131.994919999996,124.994919999996));
#26923=CARTESIAN_POINT('Origin',(505.4,132.,125.));
#26924=CARTESIAN_POINT('',(505.4,132.,-125.));
#26925=CARTESIAN_POINT('',(505.4,7.00000000000003,-1.11022170113618E-13));
#26926=CARTESIAN_POINT('',(505.4,132.,125.));
#26927=CARTESIAN_POINT('',(505.4,132.,125.));
#26928=CARTESIAN_POINT('',(505.4,132.,125.));
#26929=CARTESIAN_POINT('Origin',(480.,132.,125.));
#26930=CARTESIAN_POINT('',(479.999999999997,132.,-125.));
#26931=CARTESIAN_POINT('',(480.,132.,125.));
#26932=CARTESIAN_POINT('Origin',(487.322189922481,124.677810077519,117.67781007752));
#26933=CARTESIAN_POINT('Origin',(487.322189922481,124.677810077519,-117.67781007752));
#26934=CARTESIAN_POINT('Origin',(502.23008,-5.55111512312578E-14,-124.99492));
#26935=CARTESIAN_POINT('',(480.,-8.32667268468867E-14,-125.));
#26936=CARTESIAN_POINT('',(480.,-1.38777878078145E-13,-99.6));
#26937=CARTESIAN_POINT('',(480.,-1.38777878078145E-13,-99.6));
#26938=CARTESIAN_POINT('',(505.4,-8.32667268468867E-14,-125.));
#26939=CARTESIAN_POINT('',(480.,-8.32667268468867E-14,-125.));
#26940=CARTESIAN_POINT('',(505.4,-8.32667268468867E-14,-124.99492));
#26941=CARTESIAN_POINT('',(505.4,-8.32667268468867E-14,-125.));
#26942=CARTESIAN_POINT('',(502.23008,-1.11022302462516E-13,-121.825));
#26943=CARTESIAN_POINT('Origin',(502.23008,-5.55111512312578E-14,-124.99492));
#26944=CARTESIAN_POINT('',(487.9375,-1.11022302462516E-13,-121.825));
#26945=CARTESIAN_POINT('',(502.23008,-1.11022302462516E-13,-121.825));
#26946=CARTESIAN_POINT('',(483.175,-8.32667268468867E-14,-117.0625));
#26947=CARTESIAN_POINT('Origin',(487.9375,-1.11022302462516E-13,-117.0625));
#26948=CARTESIAN_POINT('',(483.175,-2.77555756156289E-14,-102.76992));
#26949=CARTESIAN_POINT('',(483.175,-8.32667268468867E-14,-117.0625));
#26950=CARTESIAN_POINT('',(480.00508,-1.11022302462516E-13,-99.6));
#26951=CARTESIAN_POINT('Origin',(480.00508,-1.11022302462516E-13,-102.76992));
#26952=CARTESIAN_POINT('',(480.00508,-1.11022302462516E-13,-99.6));
#26953=CARTESIAN_POINT('Origin',(480.,132.,-125.));
#26954=CARTESIAN_POINT('',(480.,132.,-125.));
#26955=CARTESIAN_POINT('',(480.,132.,-125.));
#26956=CARTESIAN_POINT('',(505.4,132.,-125.));
#26957=CARTESIAN_POINT('',(480.,132.,-125.));
#26958=CARTESIAN_POINT('',(505.4,132.,-125.));
#26959=CARTESIAN_POINT('Origin',(505.4,132.,-125.));
#26960=CARTESIAN_POINT('',(505.4,131.99492,-124.99492));
#26961=CARTESIAN_POINT('',(505.4,132.,-125.));
#26962=CARTESIAN_POINT('',(505.4,132.,-124.99492));
#26963=CARTESIAN_POINT('Origin',(502.23008,132.,-124.99492));
#26964=CARTESIAN_POINT('',(502.23008,128.825,-121.825));
#26965=CARTESIAN_POINT('Origin',(502.230080000001,131.99492,-124.99492));
#26966=CARTESIAN_POINT('',(502.23008,132.,-121.825));
#26967=CARTESIAN_POINT('Origin',(502.23008,132.,-121.825));
#26968=CARTESIAN_POINT('',(487.9375,128.825,-121.825));
#26969=CARTESIAN_POINT('',(502.23008,128.825,-121.825));
#26970=CARTESIAN_POINT('',(487.9375,132.,-121.825));
#26971=CARTESIAN_POINT('Origin',(487.9375,132.,-117.0625));
#26972=CARTESIAN_POINT('',(483.175,124.0625,-117.0625));
#26973=CARTESIAN_POINT('Origin',(487.937499999997,124.062500000003,-117.062500000003));
#26974=CARTESIAN_POINT('',(483.175,132.,-117.0625));
#26975=CARTESIAN_POINT('Origin',(483.175,132.,-117.0625));
#26976=CARTESIAN_POINT('',(483.175,109.76992,-102.76992));
#26977=CARTESIAN_POINT('',(483.175,128.03125,-121.03125));
#26978=CARTESIAN_POINT('',(483.175,132.,-102.76992));
#26979=CARTESIAN_POINT('Origin',(480.00508,132.,-102.76992));
#26980=CARTESIAN_POINT('',(480.00508,106.6,-99.6));
#26981=CARTESIAN_POINT('Origin',(480.005079999996,109.769920000005,-102.769920000005));
#26982=CARTESIAN_POINT('',(480.00508,132.,-99.6));
#26983=CARTESIAN_POINT('Origin',(480.00508,132.,-99.6));
#26984=CARTESIAN_POINT('',(480.,106.6,-99.6));
#26985=CARTESIAN_POINT('',(480.00508,106.6,-99.6));
#26986=CARTESIAN_POINT('',(480.,132.,-99.6));
#26987=CARTESIAN_POINT('Origin',(480.,132.,-99.6));
#26988=CARTESIAN_POINT('',(480.,119.3,-112.3));
#26989=CARTESIAN_POINT('Origin',(487.322189922481,124.67781007752,-117.677810077519));
#26990=CARTESIAN_POINT('Origin',(659.76992,-5.55111512312578E-14,124.99492));
#26991=CARTESIAN_POINT('',(682.,-1.11022302462516E-13,125.));
#26992=CARTESIAN_POINT('',(682.,-5.55111512312578E-14,99.6));
#26993=CARTESIAN_POINT('',(682.,-5.55111512312578E-14,99.6));
#26994=CARTESIAN_POINT('',(656.6,-5.55111512312578E-14,125.));
#26995=CARTESIAN_POINT('',(682.,-1.11022302462516E-13,125.));
#26996=CARTESIAN_POINT('',(656.6,-5.55111512312578E-14,124.99492));
#26997=CARTESIAN_POINT('',(656.6,-5.55111512312578E-14,125.));
#26998=CARTESIAN_POINT('',(659.76992,-8.32667268468867E-14,121.825));
#26999=CARTESIAN_POINT('Origin',(659.76992,-5.55111512312578E-14,124.99492));
#27000=CARTESIAN_POINT('',(674.0625,-8.32667268468867E-14,121.825));
#27001=CARTESIAN_POINT('',(659.76992,-8.32667268468867E-14,121.825));
#27002=CARTESIAN_POINT('',(678.825,-2.77555756156289E-14,117.0625));
#27003=CARTESIAN_POINT('Origin',(674.0625,-5.55111512312578E-14,117.0625));
#27004=CARTESIAN_POINT('',(678.825,-2.77555756156289E-14,102.76992));
#27005=CARTESIAN_POINT('',(678.825,-2.77555756156289E-14,117.0625));
#27006=CARTESIAN_POINT('',(681.99492,0.,99.6));
#27007=CARTESIAN_POINT('Origin',(681.99492,0.,102.76992));
#27008=CARTESIAN_POINT('',(681.99492,0.,99.6));
#27009=CARTESIAN_POINT('Origin',(682.,132.,125.));
#27010=CARTESIAN_POINT('',(682.,132.,125.));
#27011=CARTESIAN_POINT('',(682.,132.,125.));
#27012=CARTESIAN_POINT('',(656.6,132.,125.));
#27013=CARTESIAN_POINT('',(682.,132.,125.));
#27014=CARTESIAN_POINT('',(656.6,132.,125.));
#27015=CARTESIAN_POINT('Origin',(656.6,132.,125.));
#27016=CARTESIAN_POINT('',(656.6,131.99492,124.99492));
#27017=CARTESIAN_POINT('',(656.6,132.,125.));
#27018=CARTESIAN_POINT('',(656.6,132.,124.99492));
#27019=CARTESIAN_POINT('Origin',(659.76992,132.,124.99492));
#27020=CARTESIAN_POINT('',(659.76992,128.825,121.825));
#27021=CARTESIAN_POINT('Origin',(659.769919999989,131.99491999999,124.99491999999));
#27022=CARTESIAN_POINT('',(659.76992,132.,121.825));
#27023=CARTESIAN_POINT('Origin',(659.76992,132.,121.825));
#27024=CARTESIAN_POINT('',(674.0625,128.825,121.825));
#27025=CARTESIAN_POINT('',(659.76992,128.825,121.825));
#27026=CARTESIAN_POINT('',(674.0625,132.,121.825));
#27027=CARTESIAN_POINT('Origin',(674.0625,132.,117.0625));
#27028=CARTESIAN_POINT('',(678.825,124.0625,117.0625));
#27029=CARTESIAN_POINT('Origin',(674.062500000003,124.062500000003,117.062500000003));
#27030=CARTESIAN_POINT('',(678.825,132.,117.0625));
#27031=CARTESIAN_POINT('Origin',(678.825,132.,117.0625));
#27032=CARTESIAN_POINT('',(678.825,109.76992,102.76992));
#27033=CARTESIAN_POINT('',(678.825,128.03125,121.03125));
#27034=CARTESIAN_POINT('',(678.825,132.,102.76992));
#27035=CARTESIAN_POINT('Origin',(681.99492,132.,102.76992));
#27036=CARTESIAN_POINT('',(681.99492,106.6,99.6));
#27037=CARTESIAN_POINT('Origin',(681.994919999999,109.769919999999,102.769919999998));
#27038=CARTESIAN_POINT('',(681.99492,132.,99.6));
#27039=CARTESIAN_POINT('Origin',(681.99492,132.,99.6));
#27040=CARTESIAN_POINT('',(682.,106.6,99.6));
#27041=CARTESIAN_POINT('',(681.99492,106.6,99.6));
#27042=CARTESIAN_POINT('',(682.,132.,99.6));
#27043=CARTESIAN_POINT('Origin',(682.,132.,99.6));
#27044=CARTESIAN_POINT('',(682.,119.3,112.3));
#27045=CARTESIAN_POINT('Origin',(674.677810077519,124.677810077519,117.677810077519));
#27046=CARTESIAN_POINT('Origin',(682.,106.6,-125.));
#27047=CARTESIAN_POINT('',(682.000000000002,132.,-125.));
#27048=CARTESIAN_POINT('',(682.,106.6,-99.6000000000001));
#27049=CARTESIAN_POINT('',(682.,119.3,-112.3));
#27050=CARTESIAN_POINT('',(682.,132.,125.));
#27051=CARTESIAN_POINT('',(682.,132.,-125.));
#27052=CARTESIAN_POINT('',(682.,106.6,99.6000000000001));
#27053=CARTESIAN_POINT('',(681.999999999999,-5.70000000000004,-12.7));
#27054=CARTESIAN_POINT('',(682.,106.6,-125.));
#27055=CARTESIAN_POINT('Origin',(681.99492,106.6,-125.));
#27056=CARTESIAN_POINT('',(681.99492,106.6,-99.6));
#27057=CARTESIAN_POINT('',(681.99492,106.6,-99.6));
#27058=CARTESIAN_POINT('',(681.99492,106.6,99.6000000000001));
#27059=CARTESIAN_POINT('',(681.994919999999,106.6,99.6000000000001));
#27060=CARTESIAN_POINT('',(681.99492,106.6,-125.));
#27061=CARTESIAN_POINT('Origin',(681.99492,109.76992,-125.));
#27062=CARTESIAN_POINT('',(678.825,109.76992,-102.76992));
#27063=CARTESIAN_POINT('Origin',(681.994919999996,109.769919999996,-102.769919999996));
#27064=CARTESIAN_POINT('',(678.825,109.76992,102.76992));
#27065=CARTESIAN_POINT('Origin',(681.994920000006,109.769920000006,102.769920000006));
#27066=CARTESIAN_POINT('',(678.825,109.76992,-125.));
#27067=CARTESIAN_POINT('Origin',(678.825,124.0625,-125.));
#27068=CARTESIAN_POINT('',(678.825,124.0625,-117.0625));
#27069=CARTESIAN_POINT('',(678.825,128.03125,-121.03125));
#27070=CARTESIAN_POINT('',(678.825,124.0625,117.0625));
#27071=CARTESIAN_POINT('',(678.825,3.03124999999999,-3.96875000000002));
#27072=CARTESIAN_POINT('',(678.825,124.0625,-125.));
#27073=CARTESIAN_POINT('Origin',(674.0625,124.0625,-125.));
#27074=CARTESIAN_POINT('',(674.0625,128.825,-121.825));
#27075=CARTESIAN_POINT('Origin',(674.062500000007,124.062500000007,-117.062500000008));
#27076=CARTESIAN_POINT('',(674.0625,128.825,121.825));
#27077=CARTESIAN_POINT('Origin',(674.062500000002,124.062500000003,117.062500000003));
#27078=CARTESIAN_POINT('',(674.0625,128.825,-125.));
#27079=CARTESIAN_POINT('Origin',(659.76992,128.825,-125.));
#27080=CARTESIAN_POINT('',(659.76992,128.825,-121.825));
#27081=CARTESIAN_POINT('',(659.76992,128.825,-121.825));
#27082=CARTESIAN_POINT('',(659.76992,128.825,121.825));
#27083=CARTESIAN_POINT('',(659.769920000001,128.825,121.825));
#27084=CARTESIAN_POINT('',(659.76992,128.825,-125.));
#27085=CARTESIAN_POINT('Origin',(659.76992,131.99492,-125.));
#27086=CARTESIAN_POINT('',(656.6,131.99492,-124.99492));
#27087=CARTESIAN_POINT('Origin',(659.769919999996,131.994919999995,-124.994919999995));
#27088=CARTESIAN_POINT('',(656.6,131.99492,124.99492));
#27089=CARTESIAN_POINT('Origin',(659.769919999998,131.994919999999,124.99492));
#27090=CARTESIAN_POINT('',(656.6,131.99492,-125.));
#27091=CARTESIAN_POINT('Origin',(656.6,132.,-125.));
#27092=CARTESIAN_POINT('',(656.6,132.,-125.));
#27093=CARTESIAN_POINT('',(656.6,132.,-125.));
#27094=CARTESIAN_POINT('',(656.599999999998,132.,125.));
#27095=CARTESIAN_POINT('',(656.600000000001,6.99999999999999,2.77554962062901E-14));
#27096=CARTESIAN_POINT('',(656.6,132.,-125.));
#27097=CARTESIAN_POINT('Origin',(682.,132.,-125.));
#27098=CARTESIAN_POINT('',(682.,132.,-125.));
#27099=CARTESIAN_POINT('',(682.000000000001,132.,125.));
#27100=CARTESIAN_POINT('Origin',(674.677810077519,124.677810077519,117.67781007752));
#27101=CARTESIAN_POINT('Origin',(674.67781007752,124.677810077519,-117.67781007752));
#27102=CARTESIAN_POINT('Origin',(659.76992,-4.16333634234434E-14,-124.99492));
#27103=CARTESIAN_POINT('',(682.,-2.77555756156289E-14,-125.));
#27104=CARTESIAN_POINT('',(682.,-5.55111512312578E-14,-99.6));
#27105=CARTESIAN_POINT('',(682.,-5.55111512312578E-14,-99.6));
#27106=CARTESIAN_POINT('',(681.99492,-4.16333634234434E-14,-99.6));
#27107=CARTESIAN_POINT('',(681.99492,-4.16333634234434E-14,-99.6));
#27108=CARTESIAN_POINT('',(678.825,-2.77555756156289E-14,-102.76992));
#27109=CARTESIAN_POINT('Origin',(681.99492,-5.55111512312578E-14,-102.76992));
#27110=CARTESIAN_POINT('',(678.825,0.,-117.0625));
#27111=CARTESIAN_POINT('',(678.825,0.,-117.0625));
#27112=CARTESIAN_POINT('',(674.0625,-2.77555756156289E-14,-121.825));
#27113=CARTESIAN_POINT('Origin',(674.0625,-4.16333634234434E-14,-117.0625));
#27114=CARTESIAN_POINT('',(659.76992,-1.38777878078145E-14,-121.825));
#27115=CARTESIAN_POINT('',(659.76992,-1.38777878078145E-14,-121.825));
#27116=CARTESIAN_POINT('',(656.6,-1.38777878078145E-14,-124.99492));
#27117=CARTESIAN_POINT('Origin',(659.76992,-4.16333634234434E-14,-124.99492));
#27118=CARTESIAN_POINT('',(656.6,-4.16333634234434E-14,-125.));
#27119=CARTESIAN_POINT('',(656.6,-4.16333634234434E-14,-125.));
#27120=CARTESIAN_POINT('',(682.,-2.77555756156289E-14,-125.));
#27121=CARTESIAN_POINT('Origin',(682.,-2.77555756156289E-14,-125.));
#27122=CARTESIAN_POINT('',(656.6,132.,-125.));
#27123=CARTESIAN_POINT('',(656.6,-4.16333634234434E-14,-125.));
#27124=CARTESIAN_POINT('',(682.,132.,-125.));
#27125=CARTESIAN_POINT('',(682.000000000001,132.,-125.));
#27126=CARTESIAN_POINT('',(682.,-2.77555756156289E-14,-125.));
#27127=CARTESIAN_POINT('Origin',(656.6,-4.16333634234434E-14,-125.));
#27128=CARTESIAN_POINT('',(656.6,131.99492,-124.99492));
#27129=CARTESIAN_POINT('',(656.6,-1.38777878078145E-14,-124.99492));
#27130=CARTESIAN_POINT('',(656.600000000001,66.0000000000001,-59.));
#27131=CARTESIAN_POINT('Origin',(659.76992,-4.16333634234434E-14,-124.99492));
#27132=CARTESIAN_POINT('',(659.76992,128.825,-121.825));
#27133=CARTESIAN_POINT('',(659.76992,-1.38777878078145E-14,-121.825));
#27134=CARTESIAN_POINT('Origin',(659.769920000007,131.994920000008,-124.994920000007));
#27135=CARTESIAN_POINT('Origin',(659.76992,-1.38777878078145E-14,-121.825));
#27136=CARTESIAN_POINT('',(674.062500000001,128.825,-121.825));
#27137=CARTESIAN_POINT('',(674.0625,-2.77555756156289E-14,-121.825));
#27138=CARTESIAN_POINT('',(659.769920000001,128.825,-121.825));
#27139=CARTESIAN_POINT('Origin',(674.0625,-4.16333634234434E-14,-117.0625));
#27140=CARTESIAN_POINT('',(678.825,124.0625,-117.0625));
#27141=CARTESIAN_POINT('',(678.825,0.,-117.0625));
#27142=CARTESIAN_POINT('Origin',(674.0625,124.062499999999,-117.062499999999));
#27143=CARTESIAN_POINT('Origin',(678.825,0.,-117.0625));
#27144=CARTESIAN_POINT('',(678.825,109.76992,-102.76992));
#27145=CARTESIAN_POINT('',(678.825,-2.77555756156289E-14,-102.76992));
#27146=CARTESIAN_POINT('',(678.825,62.03125,-55.03125));
#27147=CARTESIAN_POINT('Origin',(681.99492,-5.55111512312578E-14,-102.76992));
#27148=CARTESIAN_POINT('',(681.99492,106.6,-99.6));
#27149=CARTESIAN_POINT('',(681.99492,-4.16333634234434E-14,-99.6));
#27150=CARTESIAN_POINT('Origin',(681.994919999999,109.769919999999,-102.769919999998));
#27151=CARTESIAN_POINT('Origin',(681.99492,-4.16333634234434E-14,-99.6));
#27152=CARTESIAN_POINT('',(682.000000000001,106.6,-99.6));
#27153=CARTESIAN_POINT('',(682.,-5.55111512312578E-14,-99.6));
#27154=CARTESIAN_POINT('',(681.99492,106.6,-99.6));
#27155=CARTESIAN_POINT('Origin',(682.,-5.55111512312578E-14,-99.6));
#27156=CARTESIAN_POINT('',(682.,53.3,-46.3));
#27157=CARTESIAN_POINT('Origin',(674.67781007752,124.67781007752,-117.677810077519));
#27158=CARTESIAN_POINT('Origin',(528.5,132.,-64.5));
#27159=CARTESIAN_POINT('',(528.5,132.,-69.));
#27160=CARTESIAN_POINT('',(528.5,132.,-60.));
#27161=CARTESIAN_POINT('Origin',(528.5,132.,-64.5));
#27162=CARTESIAN_POINT('',(528.5,140.,-69.));
#27163=CARTESIAN_POINT('',(528.5,132.,-69.));
#27164=CARTESIAN_POINT('',(528.5,140.,-60.));
#27165=CARTESIAN_POINT('Origin',(528.5,140.,-64.5));
#27166=CARTESIAN_POINT('',(528.5,132.,-60.));
#27167=CARTESIAN_POINT('Origin',(628.5,132.000000000001,-64.5));
#27168=CARTESIAN_POINT('',(628.5,132.000000000001,-69.));
#27169=CARTESIAN_POINT('',(628.5,132.000000000001,-60.));
#27170=CARTESIAN_POINT('Origin',(628.5,132.000000000001,-64.5));
#27171=CARTESIAN_POINT('',(628.5,140.000000000001,-69.));
#27172=CARTESIAN_POINT('',(628.5,132.000000000001,-69.));
#27173=CARTESIAN_POINT('',(628.5,140.000000000001,-60.));
#27174=CARTESIAN_POINT('Origin',(628.5,140.000000000001,-64.5));
#27175=CARTESIAN_POINT('',(628.5,132.000000000001,-60.));
#27176=CARTESIAN_POINT('Origin',(628.5,132.000000000001,64.5));
#27177=CARTESIAN_POINT('',(628.5,132.000000000001,60.));
#27178=CARTESIAN_POINT('',(628.5,132.000000000001,69.));
#27179=CARTESIAN_POINT('Origin',(628.5,132.000000000001,64.5));
#27180=CARTESIAN_POINT('',(628.5,140.000000000001,60.));
#27181=CARTESIAN_POINT('',(628.5,132.000000000001,60.));
#27182=CARTESIAN_POINT('',(628.5,140.000000000001,69.));
#27183=CARTESIAN_POINT('Origin',(628.5,140.000000000001,64.5));
#27184=CARTESIAN_POINT('',(628.5,132.000000000001,69.));
#27185=CARTESIAN_POINT('Origin',(528.5,132.,64.5));
#27186=CARTESIAN_POINT('',(528.5,132.,60.));
#27187=CARTESIAN_POINT('',(528.5,132.,69.));
#27188=CARTESIAN_POINT('Origin',(528.5,132.,64.5));
#27189=CARTESIAN_POINT('',(528.5,140.,60.));
#27190=CARTESIAN_POINT('',(528.5,132.,60.));
#27191=CARTESIAN_POINT('',(528.5,140.,69.));
#27192=CARTESIAN_POINT('Origin',(528.5,140.,64.5));
#27193=CARTESIAN_POINT('',(528.5,132.,69.));
#27194=CARTESIAN_POINT('Origin',(471.,140.,90.));
#27195=CARTESIAN_POINT('',(471.,132.,-79.9999999999999));
#27196=CARTESIAN_POINT('',(471.,132.,79.9999999999999));
#27197=CARTESIAN_POINT('',(471.,132.,90.));
#27198=CARTESIAN_POINT('',(471.,140.,79.9999999999999));
#27199=CARTESIAN_POINT('',(471.,140.,79.9999999999999));
#27200=CARTESIAN_POINT('',(471.,140.,-79.9999999999999));
#27201=CARTESIAN_POINT('',(471.,140.,90.));
#27202=CARTESIAN_POINT('',(471.,140.,-79.9999999999999));
#27203=CARTESIAN_POINT('Origin',(471.,140.,90.));
#27204=CARTESIAN_POINT('',(481.,140.,90.));
#27205=CARTESIAN_POINT('',(681.,140.000000000002,90.));
#27206=CARTESIAN_POINT('',(471.,140.,90.));
#27207=CARTESIAN_POINT('',(481.,132.,90.));
#27208=CARTESIAN_POINT('',(481.,140.,90.));
#27209=CARTESIAN_POINT('',(681.,132.000000000002,90.));
#27210=CARTESIAN_POINT('',(471.,132.,90.));
#27211=CARTESIAN_POINT('',(681.,140.000000000002,90.));
#27212=CARTESIAN_POINT('Origin',(691.,140.000000000002,90.));
#27213=CARTESIAN_POINT('',(691.,132.000000000002,80.));
#27214=CARTESIAN_POINT('',(691.,132.000000000002,-80.));
#27215=CARTESIAN_POINT('',(691.,132.000000000002,90.));
#27216=CARTESIAN_POINT('',(691.,140.000000000002,-80.));
#27217=CARTESIAN_POINT('',(691.,140.000000000002,-80.));
#27218=CARTESIAN_POINT('',(691.,140.000000000002,80.));
#27219=CARTESIAN_POINT('',(691.,140.000000000002,90.));
#27220=CARTESIAN_POINT('',(691.,140.000000000002,80.));
#27221=CARTESIAN_POINT('Origin',(471.,140.,-90.));
#27222=CARTESIAN_POINT('',(681.,132.000000000002,-90.));
#27223=CARTESIAN_POINT('',(481.,132.,-90.));
#27224=CARTESIAN_POINT('',(471.,132.,-90.));
#27225=CARTESIAN_POINT('',(481.,140.,-90.));
#27226=CARTESIAN_POINT('',(481.,140.,-90.));
#27227=CARTESIAN_POINT('',(681.,140.000000000002,-90.));
#27228=CARTESIAN_POINT('',(471.,140.,-90.));
#27229=CARTESIAN_POINT('',(681.,140.000000000002,-90.));
#27230=CARTESIAN_POINT('Origin',(-1.44861900253085E-12,139.999999999995,
1.05879118406788E-22));
#27231=CARTESIAN_POINT('',(481.,140.,90.));
#27232=CARTESIAN_POINT('',(691.,140.000000000002,80.));
#27233=CARTESIAN_POINT('',(681.,140.000000000002,-90.));
#27234=CARTESIAN_POINT('',(471.,140.,-79.9999999999999));
#27235=CARTESIAN_POINT('',(533.5,140.000000000001,-60.));
#27236=CARTESIAN_POINT('',(528.5,140.,-60.));
#27237=CARTESIAN_POINT('',(533.5,140.000000000001,-69.));
#27238=CARTESIAN_POINT('',(528.5,140.,-69.));
#27239=CARTESIAN_POINT('Origin',(533.5,140.000000000001,-64.5));
#27240=CARTESIAN_POINT('',(633.5,140.000000000002,-60.));
#27241=CARTESIAN_POINT('',(628.5,140.000000000001,-60.));
#27242=CARTESIAN_POINT('',(633.5,140.000000000002,-69.));
#27243=CARTESIAN_POINT('',(628.5,140.000000000001,-69.));
#27244=CARTESIAN_POINT('Origin',(633.5,140.000000000002,-64.5));
#27245=CARTESIAN_POINT('',(633.5,140.000000000002,69.));
#27246=CARTESIAN_POINT('',(628.5,140.000000000001,69.));
#27247=CARTESIAN_POINT('',(633.5,140.000000000002,60.));
#27248=CARTESIAN_POINT('',(628.5,140.000000000001,60.));
#27249=CARTESIAN_POINT('Origin',(633.5,140.000000000002,64.5));
#27250=CARTESIAN_POINT('',(533.5,140.000000000001,69.));
#27251=CARTESIAN_POINT('',(528.5,140.,69.));
#27252=CARTESIAN_POINT('',(533.5,140.000000000001,60.));
#27253=CARTESIAN_POINT('',(528.5,140.,60.));
#27254=CARTESIAN_POINT('Origin',(533.5,140.000000000001,64.5));
#27255=CARTESIAN_POINT('Origin',(-1.36557432028889E-12,131.999999999995,
0.));
#27256=CARTESIAN_POINT('',(195.500000000002,131.999999999997,-195.500000000001));
#27257=CARTESIAN_POINT('',(195.499999999998,131.999999999997,195.500000000001));
#27258=CARTESIAN_POINT('',(385.499999999998,131.999999999999,-385.500000000001));
#27259=CARTESIAN_POINT('',(385.499999999996,131.999999999999,385.500000000001));
#27260=CARTESIAN_POINT('',(533.5,132.000000000001,-60.));
#27261=CARTESIAN_POINT('',(528.5,132.,-60.));
#27262=CARTESIAN_POINT('',(533.5,132.000000000001,-69.));
#27263=CARTESIAN_POINT('Origin',(533.5,132.000000000001,-64.5));
#27264=CARTESIAN_POINT('',(528.5,132.,-69.));
#27265=CARTESIAN_POINT('',(633.5,132.000000000002,-60.));
#27266=CARTESIAN_POINT('',(628.5,132.000000000001,-60.));
#27267=CARTESIAN_POINT('',(633.5,132.000000000002,-69.));
#27268=CARTESIAN_POINT('Origin',(633.5,132.000000000002,-64.5));
#27269=CARTESIAN_POINT('',(628.5,132.000000000001,-69.));
#27270=CARTESIAN_POINT('',(633.5,132.000000000002,69.));
#27271=CARTESIAN_POINT('',(628.5,132.000000000001,69.));
#27272=CARTESIAN_POINT('',(633.5,132.000000000002,60.));
#27273=CARTESIAN_POINT('Origin',(633.5,132.000000000002,64.5));
#27274=CARTESIAN_POINT('',(628.5,132.000000000001,60.));
#27275=CARTESIAN_POINT('',(533.5,132.000000000001,69.));
#27276=CARTESIAN_POINT('',(528.5,132.,69.));
#27277=CARTESIAN_POINT('',(533.5,132.000000000001,60.));
#27278=CARTESIAN_POINT('Origin',(533.5,132.000000000001,64.5));
#27279=CARTESIAN_POINT('',(528.5,132.,60.));
#27280=CARTESIAN_POINT('Origin',(528.5,132.,60.));
#27281=CARTESIAN_POINT('',(533.5,132.000000000001,60.));
#27282=CARTESIAN_POINT('Origin',(533.5,132.000000000001,64.5));
#27283=CARTESIAN_POINT('',(533.5,132.000000000001,69.));
#27284=CARTESIAN_POINT('Origin',(528.5,132.,69.));
#27285=CARTESIAN_POINT('Origin',(628.5,132.000000000001,60.));
#27286=CARTESIAN_POINT('',(633.5,132.000000000002,60.));
#27287=CARTESIAN_POINT('Origin',(633.5,132.000000000002,64.5));
#27288=CARTESIAN_POINT('',(633.5,132.000000000002,69.));
#27289=CARTESIAN_POINT('Origin',(628.5,132.000000000001,69.));
#27290=CARTESIAN_POINT('Origin',(628.5,132.000000000001,-69.));
#27291=CARTESIAN_POINT('',(633.5,132.000000000002,-69.));
#27292=CARTESIAN_POINT('Origin',(633.5,132.000000000002,-64.5));
#27293=CARTESIAN_POINT('',(633.5,132.000000000002,-60.));
#27294=CARTESIAN_POINT('Origin',(628.5,132.000000000001,-60.));
#27295=CARTESIAN_POINT('Origin',(528.5,132.,-69.));
#27296=CARTESIAN_POINT('',(533.5,132.000000000001,-69.));
#27297=CARTESIAN_POINT('Origin',(533.5,132.000000000001,-64.5));
#27298=CARTESIAN_POINT('',(533.5,132.000000000001,-60.));
#27299=CARTESIAN_POINT('Origin',(528.5,132.,-60.));
#27300=CARTESIAN_POINT('Origin',(481.,140.,90.));
#27301=CARTESIAN_POINT('Origin',(471.,140.,-79.9999999999999));
#27302=CARTESIAN_POINT('Origin',(681.,140.000000000002,-90.));
#27303=CARTESIAN_POINT('Origin',(691.,140.000000000002,80.));
#27304=CARTESIAN_POINT('Origin',(290.,150.2,-91.9999999999992));
#27305=CARTESIAN_POINT('',(290.,143.6468,-100.749999999999));
#27306=CARTESIAN_POINT('Origin',(290.,143.6468,-91.9999999999992));
#27307=CARTESIAN_POINT('',(290.,150.2,-100.749999999999));
#27308=CARTESIAN_POINT('',(290.,150.2,-100.749999999999));
#27309=CARTESIAN_POINT('Origin',(290.,150.2,-91.9999999999992));
#27310=CARTESIAN_POINT('Origin',(290.,150.2,92.0000000000008));
#27311=CARTESIAN_POINT('',(290.,143.6468,83.2500000000008));
#27312=CARTESIAN_POINT('Origin',(290.,143.6468,92.0000000000008));
#27313=CARTESIAN_POINT('',(290.,150.2,83.2500000000008));
#27314=CARTESIAN_POINT('',(290.,150.2,83.2500000000008));
#27315=CARTESIAN_POINT('Origin',(290.,150.2,92.0000000000008));
#27316=CARTESIAN_POINT('Origin',(251.9,150.2,180.));
#27317=CARTESIAN_POINT('',(251.9,112.1508,-141.9508));
#27318=CARTESIAN_POINT('',(251.9,150.2,-180.));
#27319=CARTESIAN_POINT('',(251.900000000002,-29.8000000000002,1.11022302462516E-13));
#27320=CARTESIAN_POINT('',(251.9,112.1508,141.9508));
#27321=CARTESIAN_POINT('',(251.9,112.1508,180.));
#27322=CARTESIAN_POINT('',(251.9,150.2,180.));
#27323=CARTESIAN_POINT('',(251.9,150.2,180.));
#27324=CARTESIAN_POINT('',(251.9,150.2,180.));
#27325=CARTESIAN_POINT('Origin',(251.9,112.1508,180.));
#27326=CARTESIAN_POINT('',(254.057664864162,112.1508,-141.9508));
#27327=CARTESIAN_POINT('',(251.9,112.1508,-141.9508));
#27328=CARTESIAN_POINT('',(254.057664864162,112.1508,141.9508));
#27329=CARTESIAN_POINT('',(254.057664864162,112.1508,180.));
#27330=CARTESIAN_POINT('',(251.9,112.1508,141.9508));
#27331=CARTESIAN_POINT('Origin',(254.057664864162,114.6908,180.));
#27332=CARTESIAN_POINT('',(256.563100490752,114.273196933659,-144.073196933659));
#27333=CARTESIAN_POINT('Origin',(254.057664864164,114.690799999998,-144.490799999998));
#27334=CARTESIAN_POINT('',(256.563100490752,114.273196933659,144.073196933659));
#27335=CARTESIAN_POINT('',(256.563100490752,114.273196933659,180.));
#27336=CARTESIAN_POINT('Origin',(254.05766486416,114.690800000002,144.490800000002));
#27337=CARTESIAN_POINT('Origin',(260.503909842616,137.916328279119,180.));
#27338=CARTESIAN_POINT('',(260.503909842617,137.916328279119,-167.71632827912));
#27339=CARTESIAN_POINT('',(231.92245785816,-33.5598744437294,3.75987444372938));
#27340=CARTESIAN_POINT('',(260.503909842617,137.916328279119,167.716328279119));
#27341=CARTESIAN_POINT('',(260.503909842617,137.916328279119,180.));
#27342=CARTESIAN_POINT('',(261.51359832984,143.974017294229,173.774017294229));
#27343=CARTESIAN_POINT('Origin',(267.268586034408,136.7888,180.));
#27344=CARTESIAN_POINT('',(267.268586034408,143.6468,-173.4468));
#27345=CARTESIAN_POINT('Origin',(267.268586034408,136.788799999999,-166.588799999999));
#27346=CARTESIAN_POINT('',(267.268586034408,143.6468,173.4468));
#27347=CARTESIAN_POINT('',(267.268586034408,143.6468,180.));
#27348=CARTESIAN_POINT('Origin',(267.268586034408,136.788799999999,166.5888));
#27349=CARTESIAN_POINT('Origin',(312.731413965592,143.6468,180.));
#27350=CARTESIAN_POINT('',(312.731413965592,143.6468,-173.4468));
#27351=CARTESIAN_POINT('',(312.731413965589,143.6468,-173.4468));
#27352=CARTESIAN_POINT('',(312.731413965592,143.6468,173.4468));
#27353=CARTESIAN_POINT('',(312.731413965592,143.6468,180.));
#27354=CARTESIAN_POINT('',(312.731413965592,143.6468,173.4468));
#27355=CARTESIAN_POINT('Origin',(312.731413965592,136.7888,180.));
#27356=CARTESIAN_POINT('',(319.496090157384,137.91632827912,-167.71632827912));
#27357=CARTESIAN_POINT('Origin',(312.731413965593,136.788800000001,-166.588800000001));
#27358=CARTESIAN_POINT('',(319.496090157384,137.91632827912,167.71632827912));
#27359=CARTESIAN_POINT('',(319.496090157384,137.91632827912,180.));
#27360=CARTESIAN_POINT('Origin',(312.731413965592,136.788799999999,166.588799999999));
#27361=CARTESIAN_POINT('Origin',(319.496090157384,137.91632827912,180.));
#27362=CARTESIAN_POINT('',(323.436899509249,114.27319693366,-144.07319693366));
#27363=CARTESIAN_POINT('',(348.077542141844,-33.5598744437285,3.75987444372849));
#27364=CARTESIAN_POINT('',(323.436899509249,114.27319693366,144.07319693366));
#27365=CARTESIAN_POINT('',(323.436899509249,114.27319693366,180.));
#27366=CARTESIAN_POINT('',(318.48640167016,143.974017294229,173.774017294229));
#27367=CARTESIAN_POINT('Origin',(325.942335135838,114.6908,180.));
#27368=CARTESIAN_POINT('',(325.942335135838,112.1508,-141.9508));
#27369=CARTESIAN_POINT('Origin',(325.942335135832,114.690799999993,-144.490799999993));
#27370=CARTESIAN_POINT('',(325.942335135838,112.1508,141.9508));
#27371=CARTESIAN_POINT('',(325.942335135838,112.1508,180.));
#27372=CARTESIAN_POINT('Origin',(325.942335135844,114.690800000007,144.490800000007));
#27373=CARTESIAN_POINT('Origin',(328.1,112.1508,180.));
#27374=CARTESIAN_POINT('',(328.1,112.1508,-141.9508));
#27375=CARTESIAN_POINT('',(328.1,112.1508,-141.9508));
#27376=CARTESIAN_POINT('',(328.1,112.1508,141.9508));
#27377=CARTESIAN_POINT('',(328.1,112.1508,180.));
#27378=CARTESIAN_POINT('',(328.1,112.1508,141.9508));
#27379=CARTESIAN_POINT('Origin',(328.1,150.2,180.));
#27380=CARTESIAN_POINT('',(328.1,150.2,-180.));
#27381=CARTESIAN_POINT('',(328.100000000002,-29.7999999999998,-2.4980018054066E-13));
#27382=CARTESIAN_POINT('',(328.1,150.2,180.));
#27383=CARTESIAN_POINT('',(328.1,150.2,180.));
#27384=CARTESIAN_POINT('',(328.1,150.2,180.));
#27385=CARTESIAN_POINT('Origin',(251.9,150.2,180.));
#27386=CARTESIAN_POINT('',(251.899999999996,150.2,-180.));
#27387=CARTESIAN_POINT('',(251.9,150.2,180.));
#27388=CARTESIAN_POINT('Origin',(290.,139.06874412503,168.86874412503));
#27389=CARTESIAN_POINT('Origin',(290.,139.06874412503,-168.86874412503));
#27390=CARTESIAN_POINT('Origin',(45.,80.0050800000034,169.));
#27391=CARTESIAN_POINT('',(45.,76.83008,164.5));
#27392=CARTESIAN_POINT('Origin',(45.,76.8300800000001,169.));
#27393=CARTESIAN_POINT('',(45.,80.0050800000034,164.5));
#27394=CARTESIAN_POINT('',(45.,80.0050800000034,164.5));
#27395=CARTESIAN_POINT('Origin',(45.,80.0050800000034,169.));
#27396=CARTESIAN_POINT('Origin',(175.,80.0050800000034,169.));
#27397=CARTESIAN_POINT('',(175.,76.83008,164.5));
#27398=CARTESIAN_POINT('Origin',(175.,76.8300800000001,169.));
#27399=CARTESIAN_POINT('',(175.,80.0050800000034,164.5));
#27400=CARTESIAN_POINT('',(175.,80.0050800000034,164.5));
#27401=CARTESIAN_POINT('Origin',(175.,80.0050800000034,169.));
#27402=CARTESIAN_POINT('Origin',(210.,80.00508,180.));
#27403=CARTESIAN_POINT('',(10.,80.0050800000003,154.6));
#27404=CARTESIAN_POINT('',(10.,80.00508,180.));
#27405=CARTESIAN_POINT('',(10.,80.00508,180.));
#27406=CARTESIAN_POINT('',(210.,80.00508,180.));
#27407=CARTESIAN_POINT('',(210.,80.00508,180.));
#27408=CARTESIAN_POINT('',(210.,80.0050800000003,154.6));
#27409=CARTESIAN_POINT('',(210.,80.00508,180.));
#27410=CARTESIAN_POINT('',(210.,80.0050800000003,154.6));
#27411=CARTESIAN_POINT('Origin',(210.,80.,180.));
#27412=CARTESIAN_POINT('',(10.,80.,180.));
#27413=CARTESIAN_POINT('',(10.,80.,180.));
#27414=CARTESIAN_POINT('',(210.,80.,180.));
#27415=CARTESIAN_POINT('',(210.,80.,180.));
#27416=CARTESIAN_POINT('',(210.,80.,180.));
#27417=CARTESIAN_POINT('Origin',(210.,80.0000000000001,176.83008));
#27418=CARTESIAN_POINT('',(10.,76.8300800000001,176.83008));
#27419=CARTESIAN_POINT('Origin',(10.,80.0000000000001,176.83008));
#27420=CARTESIAN_POINT('',(210.,76.8300800000001,176.83008));
#27421=CARTESIAN_POINT('',(210.,76.8300800000001,176.83008));
#27422=CARTESIAN_POINT('Origin',(210.,80.0000000000001,176.83008));
#27423=CARTESIAN_POINT('Origin',(210.,76.8300800000002,162.5375));
#27424=CARTESIAN_POINT('',(10.,76.8300800000002,162.5375));
#27425=CARTESIAN_POINT('',(10.,76.8300800000002,162.5375));
#27426=CARTESIAN_POINT('',(210.,76.8300800000002,162.5375));
#27427=CARTESIAN_POINT('',(210.,76.8300800000002,162.5375));
#27428=CARTESIAN_POINT('',(210.,76.8300800000002,162.5375));
#27429=CARTESIAN_POINT('Origin',(210.,72.0675800000002,162.5375));
#27430=CARTESIAN_POINT('',(10.,72.0675800000002,157.775));
#27431=CARTESIAN_POINT('Origin',(10.,72.0675800000002,162.5375));
#27432=CARTESIAN_POINT('',(210.,72.0675800000002,157.775));
#27433=CARTESIAN_POINT('',(210.,72.0675800000002,157.775));
#27434=CARTESIAN_POINT('Origin',(210.,72.0675800000002,162.5375));
#27435=CARTESIAN_POINT('Origin',(210.,57.7750000000002,157.775));
#27436=CARTESIAN_POINT('',(10.,57.7750000000002,157.775));
#27437=CARTESIAN_POINT('',(10.,57.7750000000002,157.775));
#27438=CARTESIAN_POINT('',(210.,57.7750000000002,157.775));
#27439=CARTESIAN_POINT('',(210.,57.7750000000002,157.775));
#27440=CARTESIAN_POINT('',(210.,57.7750000000002,157.775));
#27441=CARTESIAN_POINT('Origin',(210.,57.7750000000002,154.60508));
#27442=CARTESIAN_POINT('',(10.,54.6050800000003,154.60508));
#27443=CARTESIAN_POINT('Origin',(10.,57.7750000000002,154.60508));
#27444=CARTESIAN_POINT('',(210.,54.6050800000003,154.60508));
#27445=CARTESIAN_POINT('',(210.,54.6050800000003,154.60508));
#27446=CARTESIAN_POINT('Origin',(210.,57.7750000000002,154.60508));
#27447=CARTESIAN_POINT('Origin',(210.,54.6050800000003,154.6));
#27448=CARTESIAN_POINT('',(10.,54.6050800000003,154.6));
#27449=CARTESIAN_POINT('',(10.,54.6050800000003,154.6));
#27450=CARTESIAN_POINT('',(210.,54.6050800000003,154.6));
#27451=CARTESIAN_POINT('',(210.,54.6050800000003,154.6));
#27452=CARTESIAN_POINT('',(210.,54.6050800000003,154.6));
#27453=CARTESIAN_POINT('Origin',(210.,80.0050800000003,154.6));
#27454=CARTESIAN_POINT('',(10.,80.0050800000003,154.6));
#27455=CARTESIAN_POINT('',(210.,80.0050800000003,154.6));
#27456=CARTESIAN_POINT('Origin',(210.,57.7750000000002,154.60508));
#27457=CARTESIAN_POINT('Origin',(10.,57.7750000000002,154.60508));
#27458=CARTESIAN_POINT('Origin',(45.,80.0050800000001,-169.));
#27459=CARTESIAN_POINT('',(45.,76.8300800000001,-173.5));
#27460=CARTESIAN_POINT('Origin',(45.,76.8300800000001,-169.));
#27461=CARTESIAN_POINT('',(45.,80.0050800000001,-173.5));
#27462=CARTESIAN_POINT('',(45.,80.0050800000001,-173.5));
#27463=CARTESIAN_POINT('Origin',(45.,80.0050800000001,-169.));
#27464=CARTESIAN_POINT('Origin',(175.,80.0050800000001,-169.));
#27465=CARTESIAN_POINT('',(175.,76.8300800000001,-173.5));
#27466=CARTESIAN_POINT('Origin',(175.,76.8300800000001,-169.));
#27467=CARTESIAN_POINT('',(175.,80.0050800000001,-173.5));
#27468=CARTESIAN_POINT('',(175.,80.0050800000001,-173.5));
#27469=CARTESIAN_POINT('Origin',(175.,80.0050800000001,-169.));
#27470=CARTESIAN_POINT('Origin',(210.,80.00508,-180.));
#27471=CARTESIAN_POINT('',(10.,80.0050800000003,-154.6));
#27472=CARTESIAN_POINT('',(10.,80.00508,-180.));
#27473=CARTESIAN_POINT('',(10.,80.00508,-180.));
#27474=CARTESIAN_POINT('',(210.,80.0050800000003,-154.6));
#27475=CARTESIAN_POINT('',(210.,80.0050800000003,-154.6));
#27476=CARTESIAN_POINT('',(210.,80.00508,-180.));
#27477=CARTESIAN_POINT('',(210.,80.00508,-180.));
#27478=CARTESIAN_POINT('',(210.,80.00508,-180.));
#27479=CARTESIAN_POINT('Origin',(210.,80.,-180.));
#27480=CARTESIAN_POINT('',(10.,80.,-180.));
#27481=CARTESIAN_POINT('',(10.,80.,-180.));
#27482=CARTESIAN_POINT('',(210.,80.,-180.));
#27483=CARTESIAN_POINT('',(210.,80.,-180.));
#27484=CARTESIAN_POINT('',(210.,80.,-180.));
#27485=CARTESIAN_POINT('Origin',(210.,80.0000000000001,-176.83008));
#27486=CARTESIAN_POINT('',(10.,76.8300800000001,-176.83008));
#27487=CARTESIAN_POINT('Origin',(10.,80.0000000000001,-176.83008));
#27488=CARTESIAN_POINT('',(210.,76.8300800000001,-176.83008));
#27489=CARTESIAN_POINT('Origin',(210.,80.0000000000001,-176.83008));
#27490=CARTESIAN_POINT('',(210.,76.8300800000001,-176.83008));
#27491=CARTESIAN_POINT('Origin',(210.,76.8300800000002,-162.5375));
#27492=CARTESIAN_POINT('',(10.,76.8300800000002,-162.5375));
#27493=CARTESIAN_POINT('',(10.,76.8300800000002,-162.5375));
#27494=CARTESIAN_POINT('',(210.,76.8300800000002,-162.5375));
#27495=CARTESIAN_POINT('',(210.,76.8300800000002,-162.5375));
#27496=CARTESIAN_POINT('',(210.,76.8300800000002,-162.5375));
#27497=CARTESIAN_POINT('Origin',(210.,72.0675800000002,-162.5375));
#27498=CARTESIAN_POINT('',(10.,72.0675800000002,-157.775));
#27499=CARTESIAN_POINT('Origin',(10.,72.0675800000002,-162.5375));
#27500=CARTESIAN_POINT('',(210.,72.0675800000002,-157.775));
#27501=CARTESIAN_POINT('Origin',(210.,72.0675800000002,-162.5375));
#27502=CARTESIAN_POINT('',(210.,72.0675800000002,-157.775));
#27503=CARTESIAN_POINT('Origin',(210.,57.7750000000002,-157.775));
#27504=CARTESIAN_POINT('',(10.,57.7750000000002,-157.775));
#27505=CARTESIAN_POINT('',(10.,57.7750000000002,-157.775));
#27506=CARTESIAN_POINT('',(210.,57.7750000000002,-157.775));
#27507=CARTESIAN_POINT('',(210.,57.7750000000002,-157.775));
#27508=CARTESIAN_POINT('',(210.,57.7750000000002,-157.775));
#27509=CARTESIAN_POINT('Origin',(210.,57.7750000000002,-154.60508));
#27510=CARTESIAN_POINT('',(10.,54.6050800000003,-154.60508));
#27511=CARTESIAN_POINT('Origin',(10.,57.7750000000002,-154.60508));
#27512=CARTESIAN_POINT('',(210.,54.6050800000003,-154.60508));
#27513=CARTESIAN_POINT('Origin',(210.,57.7750000000002,-154.60508));
#27514=CARTESIAN_POINT('',(210.,54.6050800000003,-154.60508));
#27515=CARTESIAN_POINT('Origin',(210.,54.6050800000003,-154.6));
#27516=CARTESIAN_POINT('',(10.,54.6050800000003,-154.6));
#27517=CARTESIAN_POINT('',(10.,54.6050800000003,-154.6));
#27518=CARTESIAN_POINT('',(210.,54.6050800000003,-154.6));
#27519=CARTESIAN_POINT('',(210.,54.6050800000003,-154.6));
#27520=CARTESIAN_POINT('',(210.,54.6050800000003,-154.6));
#27521=CARTESIAN_POINT('Origin',(210.,80.0050800000003,-154.6));
#27522=CARTESIAN_POINT('',(10.,80.0050800000003,-154.6));
#27523=CARTESIAN_POINT('',(210.,80.0050800000003,-154.6));
#27524=CARTESIAN_POINT('Origin',(210.,57.7750000000002,-154.60508));
#27525=CARTESIAN_POINT('Origin',(10.,57.7750000000002,-154.60508));
#27526=CARTESIAN_POINT('',(229.509866214357,539.202526002623,-83.8913917541518));
#27527=CARTESIAN_POINT('',(455.009866214357,539.202526002625,-83.8913917541401));
#27528=CARTESIAN_POINT('',(104.509866214357,539.202526002623,-83.891391754152));
#27529=CARTESIAN_POINT('',(119.509866214357,319.197446002625,-83.8913917541504));
#27530=UNCERTAINTY_MEASURE_WITH_UNIT(LENGTH_MEASURE(0.01),#27542,
'DISTANCE_ACCURACY_VALUE',
'Maximum model space distance between geometric entities at asserted c
onnectivities');
#27531=UNCERTAINTY_MEASURE_WITH_UNIT(LENGTH_MEASURE(0.01),#27542,
'DISTANCE_ACCURACY_VALUE',
'Maximum model space distance between geometric entities at asserted c
onnectivities');
#27532=UNCERTAINTY_MEASURE_WITH_UNIT(LENGTH_MEASURE(0.01),#27542,
'DISTANCE_ACCURACY_VALUE',
'Maximum model space distance between geometric entities at asserted c
onnectivities');
#27533=UNCERTAINTY_MEASURE_WITH_UNIT(LENGTH_MEASURE(0.01),#27542,
'DISTANCE_ACCURACY_VALUE',
'Maximum model space distance between geometric entities at asserted c
onnectivities');
#27534=UNCERTAINTY_MEASURE_WITH_UNIT(LENGTH_MEASURE(0.01),#27542,
'DISTANCE_ACCURACY_VALUE',
'Maximum model space distance between geometric entities at asserted c
onnectivities');
#27535=UNCERTAINTY_MEASURE_WITH_UNIT(LENGTH_MEASURE(0.01),#27542,
'DISTANCE_ACCURACY_VALUE',
'Maximum model space distance between geometric entities at asserted c
onnectivities');
#27536=(
GEOMETRIC_REPRESENTATION_CONTEXT(3)
GLOBAL_UNCERTAINTY_ASSIGNED_CONTEXT((#27530))
GLOBAL_UNIT_ASSIGNED_CONTEXT((#27542,#27544,#27545))
REPRESENTATION_CONTEXT('','3D')
);
#27537=(
GEOMETRIC_REPRESENTATION_CONTEXT(3)
GLOBAL_UNCERTAINTY_ASSIGNED_CONTEXT((#27531))
GLOBAL_UNIT_ASSIGNED_CONTEXT((#27542,#27544,#27545))
REPRESENTATION_CONTEXT('','3D')
);
#27538=(
GEOMETRIC_REPRESENTATION_CONTEXT(3)
GLOBAL_UNCERTAINTY_ASSIGNED_CONTEXT((#27532))
GLOBAL_UNIT_ASSIGNED_CONTEXT((#27542,#27544,#27545))
REPRESENTATION_CONTEXT('','3D')
);
#27539=(
GEOMETRIC_REPRESENTATION_CONTEXT(3)
GLOBAL_UNCERTAINTY_ASSIGNED_CONTEXT((#27533))
GLOBAL_UNIT_ASSIGNED_CONTEXT((#27542,#27544,#27545))
REPRESENTATION_CONTEXT('','3D')
);
#27540=(
GEOMETRIC_REPRESENTATION_CONTEXT(3)
GLOBAL_UNCERTAINTY_ASSIGNED_CONTEXT((#27534))
GLOBAL_UNIT_ASSIGNED_CONTEXT((#27542,#27544,#27545))
REPRESENTATION_CONTEXT('','3D')
);
#27541=(
GEOMETRIC_REPRESENTATION_CONTEXT(3)
GLOBAL_UNCERTAINTY_ASSIGNED_CONTEXT((#27535))
GLOBAL_UNIT_ASSIGNED_CONTEXT((#27542,#27544,#27545))
REPRESENTATION_CONTEXT('','3D')
);
#27542=(
LENGTH_UNIT()
NAMED_UNIT(*)
SI_UNIT(.MILLI.,.METRE.)
);
#27543=(
LENGTH_UNIT()
NAMED_UNIT(*)
SI_UNIT($,.METRE.)
);
#27544=(
NAMED_UNIT(*)
PLANE_ANGLE_UNIT()
SI_UNIT($,.RADIAN.)
);
#27545=(
NAMED_UNIT(*)
SI_UNIT($,.STERADIAN.)
SOLID_ANGLE_UNIT()
);
#27546=SHAPE_DEFINITION_REPRESENTATION(#27551,#27560);
#27547=SHAPE_DEFINITION_REPRESENTATION(#27552,#27561);
#27548=SHAPE_DEFINITION_REPRESENTATION(#27553,#27562);
#27549=SHAPE_DEFINITION_REPRESENTATION(#27554,#27563);
#27550=SHAPE_DEFINITION_REPRESENTATION(#27555,#27564);
#27551=PRODUCT_DEFINITION_SHAPE('',$,#27566);
#27552=PRODUCT_DEFINITION_SHAPE('',$,#27567);
#27553=PRODUCT_DEFINITION_SHAPE('',$,#27568);
#27554=PRODUCT_DEFINITION_SHAPE('',$,#27569);
#27555=PRODUCT_DEFINITION_SHAPE('',$,#27570);
#27556=PRODUCT_DEFINITION_SHAPE($,$,#23);
#27557=PRODUCT_DEFINITION_SHAPE($,$,#24);
#27558=PRODUCT_DEFINITION_SHAPE($,$,#25);
#27559=PRODUCT_DEFINITION_SHAPE($,$,#26);
#27560=SHAPE_REPRESENTATION('',(#11895,#13173,#13174,#13175,#13176),#27536);
#27561=SHAPE_REPRESENTATION('',(#11896),#27537);
#27562=SHAPE_REPRESENTATION('',(#12424),#27538);
#27563=SHAPE_REPRESENTATION('',(#12619),#27539);
#27564=SHAPE_REPRESENTATION('',(#12666),#27540);
#27565=PRODUCT_DEFINITION_CONTEXT('part definition',#27582,'design');
#27566=PRODUCT_DEFINITION('MAT-021','MAT-021',#27571,#27565);
#27567=PRODUCT_DEFINITION('1. Housing','1. Housing',#27572,#27565);
#27568=PRODUCT_DEFINITION('2. Impeller','2. Impeller',#27573,#27565);
#27569=PRODUCT_DEFINITION('3. Flange','3. Flange',#27574,#27565);
#27570=PRODUCT_DEFINITION('4. Frame','4. Frame',#27575,#27565);
#27571=PRODUCT_DEFINITION_FORMATION('',$,#27584);
#27572=PRODUCT_DEFINITION_FORMATION('',$,#27585);
#27573=PRODUCT_DEFINITION_FORMATION('',$,#27586);
#27574=PRODUCT_DEFINITION_FORMATION('',$,#27587);
#27575=PRODUCT_DEFINITION_FORMATION('',$,#27588);
#27576=PRODUCT_RELATED_PRODUCT_CATEGORY('MAT-021','MAT-021',(#27584));
#27577=PRODUCT_RELATED_PRODUCT_CATEGORY('1. Housing','1. Housing',(#27585));
#27578=PRODUCT_RELATED_PRODUCT_CATEGORY('2. Impeller','2. Impeller',(#27586));
#27579=PRODUCT_RELATED_PRODUCT_CATEGORY('3. Flange','3. Flange',(#27587));
#27580=PRODUCT_RELATED_PRODUCT_CATEGORY('4. Frame','4. Frame',(#27588));
#27581=APPLICATION_PROTOCOL_DEFINITION('international standard',
'automotive_design',2009,#27582);
#27582=APPLICATION_CONTEXT(
'Core Data for Automotive Mechanical Design Process');
#27583=PRODUCT_CONTEXT('part definition',#27582,'mechanical');
#27584=PRODUCT('MAT-021','MAT-021','STEP AP214',(#27583));
#27585=PRODUCT('1. Housing','1. Housing',$,(#27583));
#27586=PRODUCT('2. Impeller','2. Impeller',$,(#27583));
#27587=PRODUCT('3. Flange','3. Flange',$,(#27583));
#27588=PRODUCT('4. Frame','4. Frame',$,(#27583));
#27589=PRESENTATION_STYLE_ASSIGNMENT((#27593));
#27590=PRESENTATION_STYLE_ASSIGNMENT((#27594));
#27591=PRESENTATION_STYLE_ASSIGNMENT((#27595));
#27592=PRESENTATION_STYLE_ASSIGNMENT((#27596));
#27593=SURFACE_STYLE_USAGE(.BOTH.,#27597);
#27594=SURFACE_STYLE_USAGE(.BOTH.,#27598);
#27595=SURFACE_STYLE_USAGE(.BOTH.,#27599);
#27596=SURFACE_STYLE_USAGE(.BOTH.,#27600);
#27597=SURFACE_SIDE_STYLE('',(#27601));
#27598=SURFACE_SIDE_STYLE('',(#27602));
#27599=SURFACE_SIDE_STYLE('',(#27603));
#27600=SURFACE_SIDE_STYLE('',(#27604));
#27601=SURFACE_STYLE_FILL_AREA(#27605);
#27602=SURFACE_STYLE_FILL_AREA(#27606);
#27603=SURFACE_STYLE_FILL_AREA(#27607);
#27604=SURFACE_STYLE_FILL_AREA(#27608);
#27605=FILL_AREA_STYLE('Steel - Satin',(#27609));
#27606=FILL_AREA_STYLE('Opaque(20,51,87)',(#27610));
#27607=FILL_AREA_STYLE('Opaque(227,224,212)',(#27611));
#27608=FILL_AREA_STYLE('Opaque(97,158,199)',(#27612));
#27609=FILL_AREA_STYLE_COLOUR('Steel - Satin',#27613);
#27610=FILL_AREA_STYLE_COLOUR('Opaque(20,51,87)',#27614);
#27611=FILL_AREA_STYLE_COLOUR('Opaque(227,224,212)',#27615);
#27612=FILL_AREA_STYLE_COLOUR('Opaque(97,158,199)',#27616);
#27613=COLOUR_RGB('Steel - Satin',0.627450980392157,0.627450980392157,0.627450980392157);
#27614=COLOUR_RGB('Opaque(20,51,87)',0.0784313725490196,0.2,0.341176470588235);
#27615=COLOUR_RGB('Opaque(227,224,212)',0.890196078431372,0.87843137254902,
0.831372549019608);
#27616=COLOUR_RGB('Opaque(97,158,199)',0.380392156862745,0.619607843137255,
0.780392156862745);
ENDSEC;
END-ISO-10303-21;
